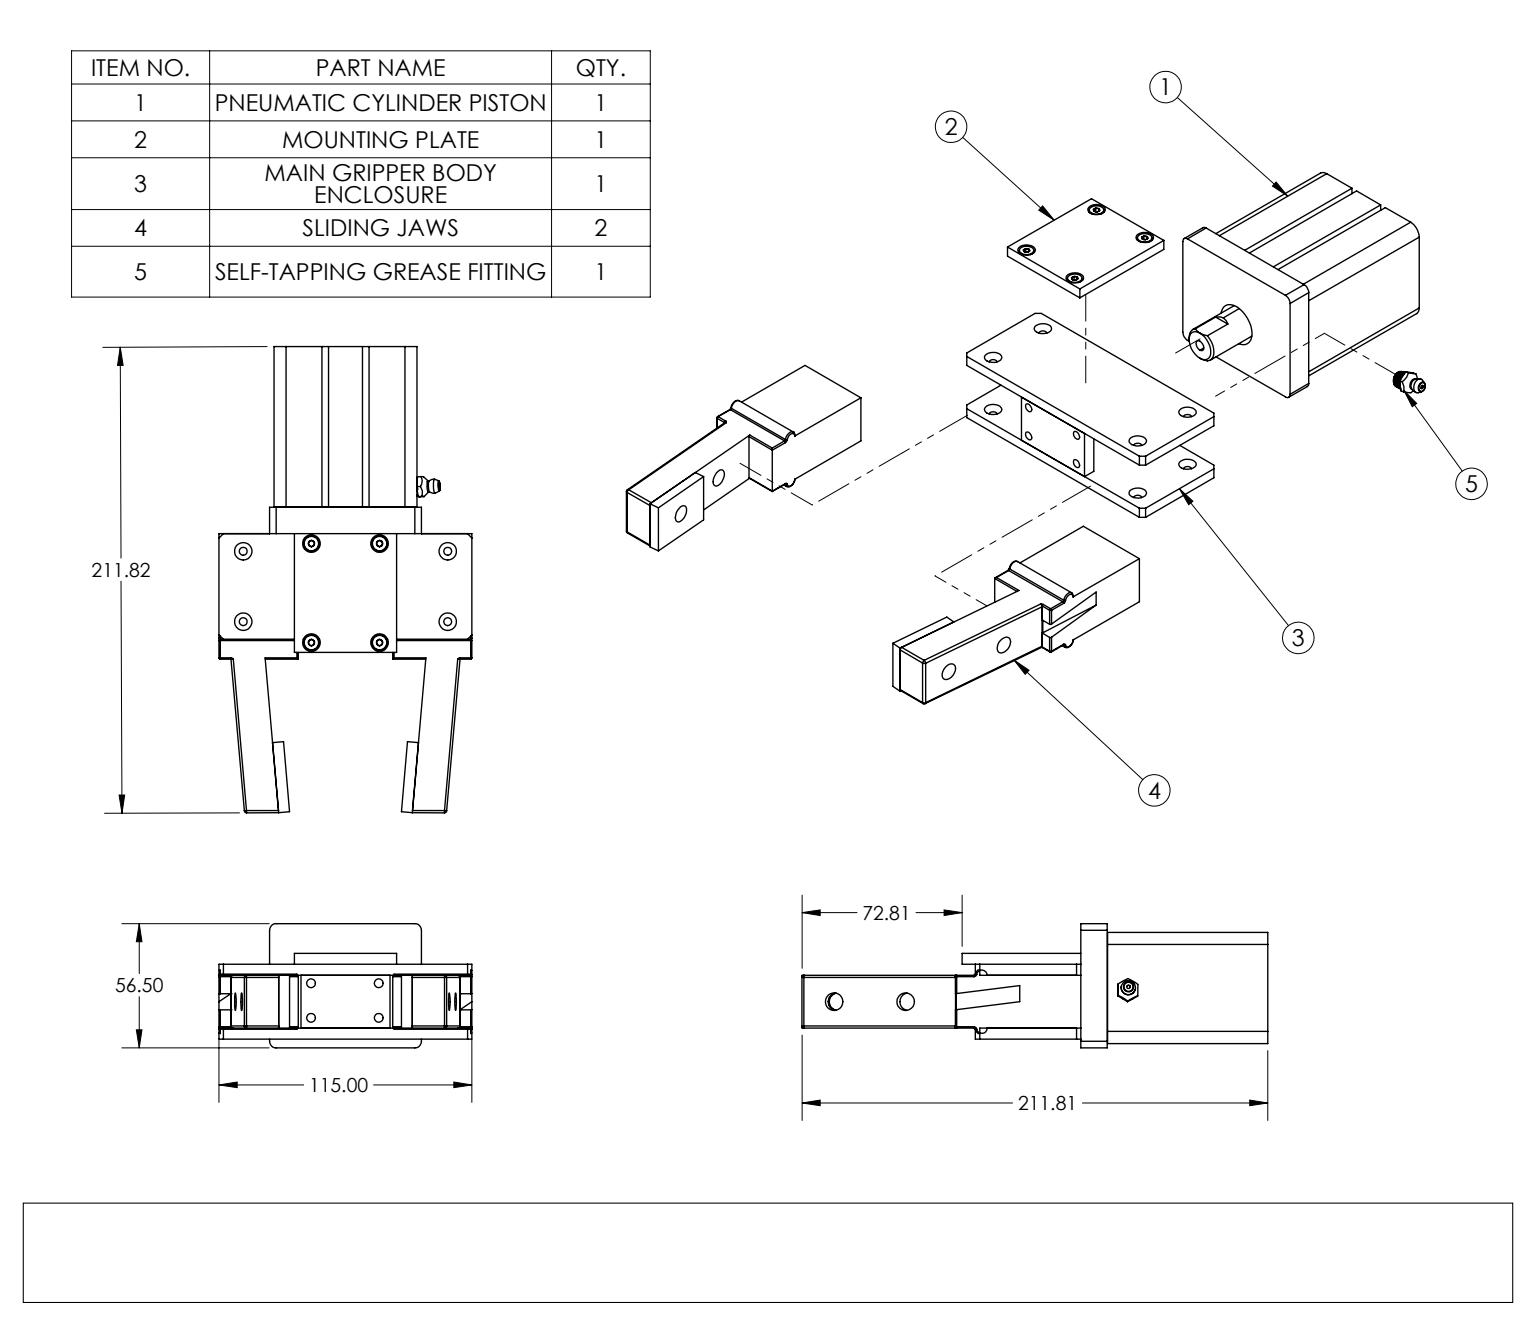
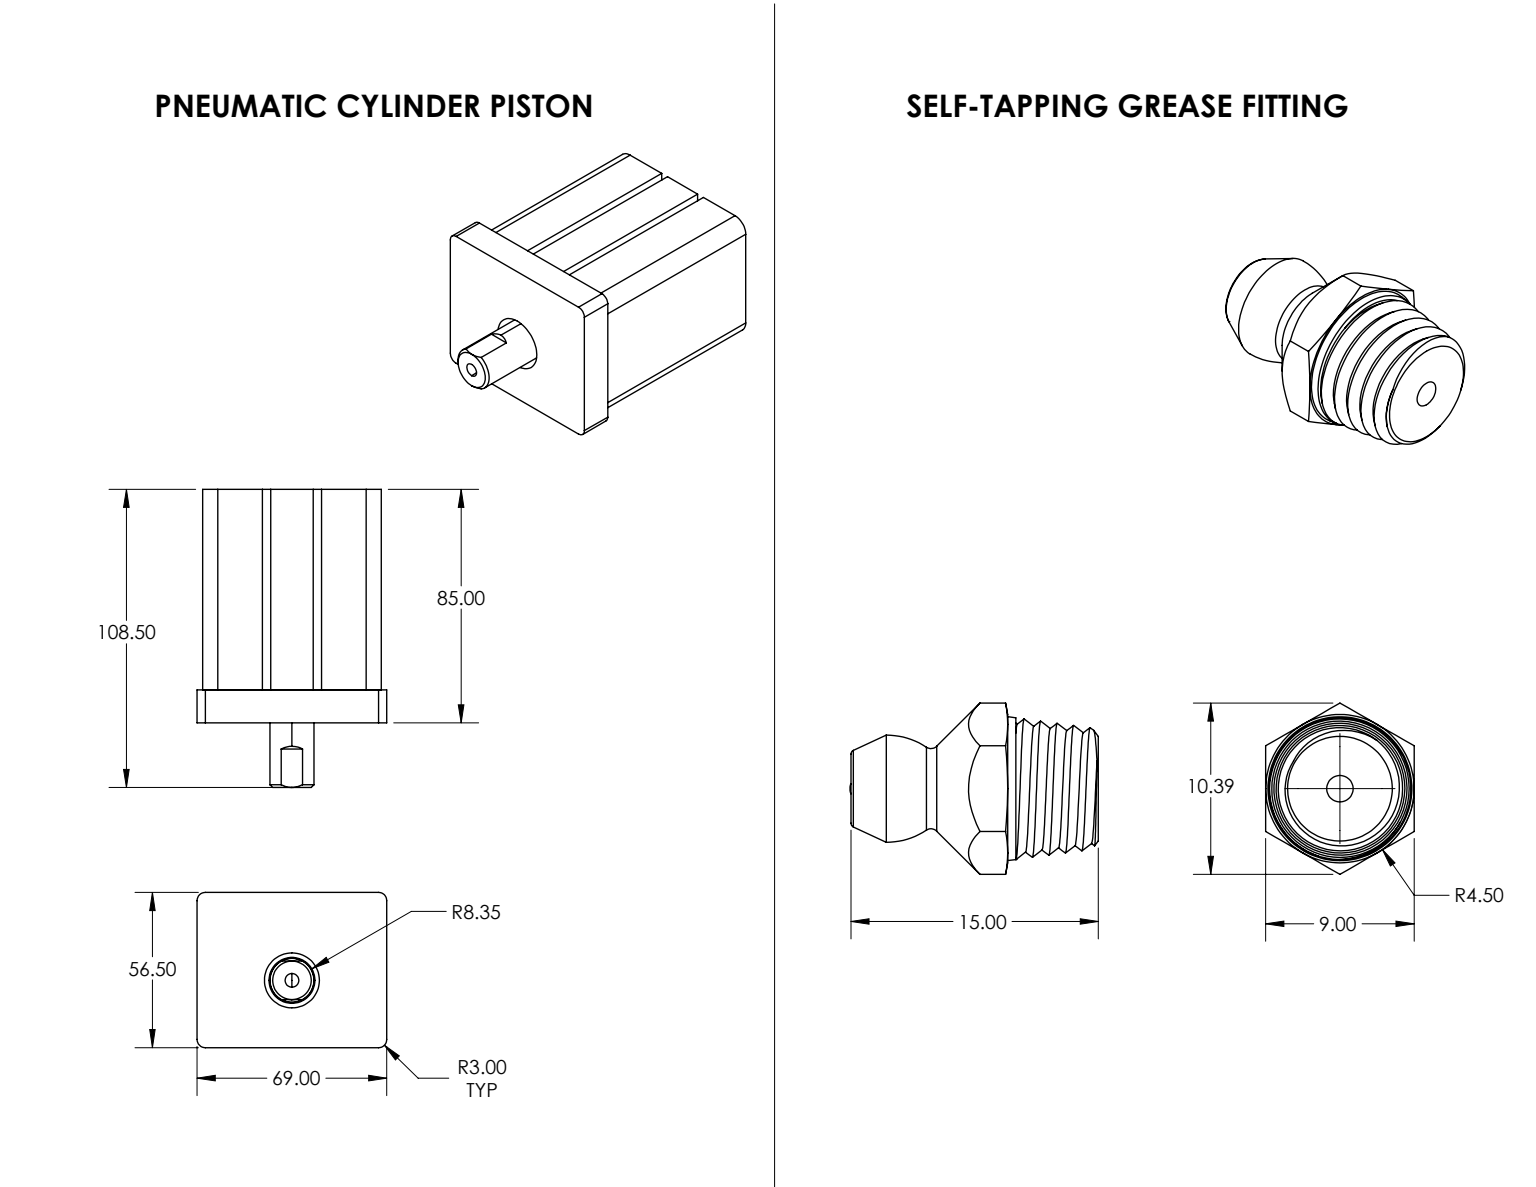
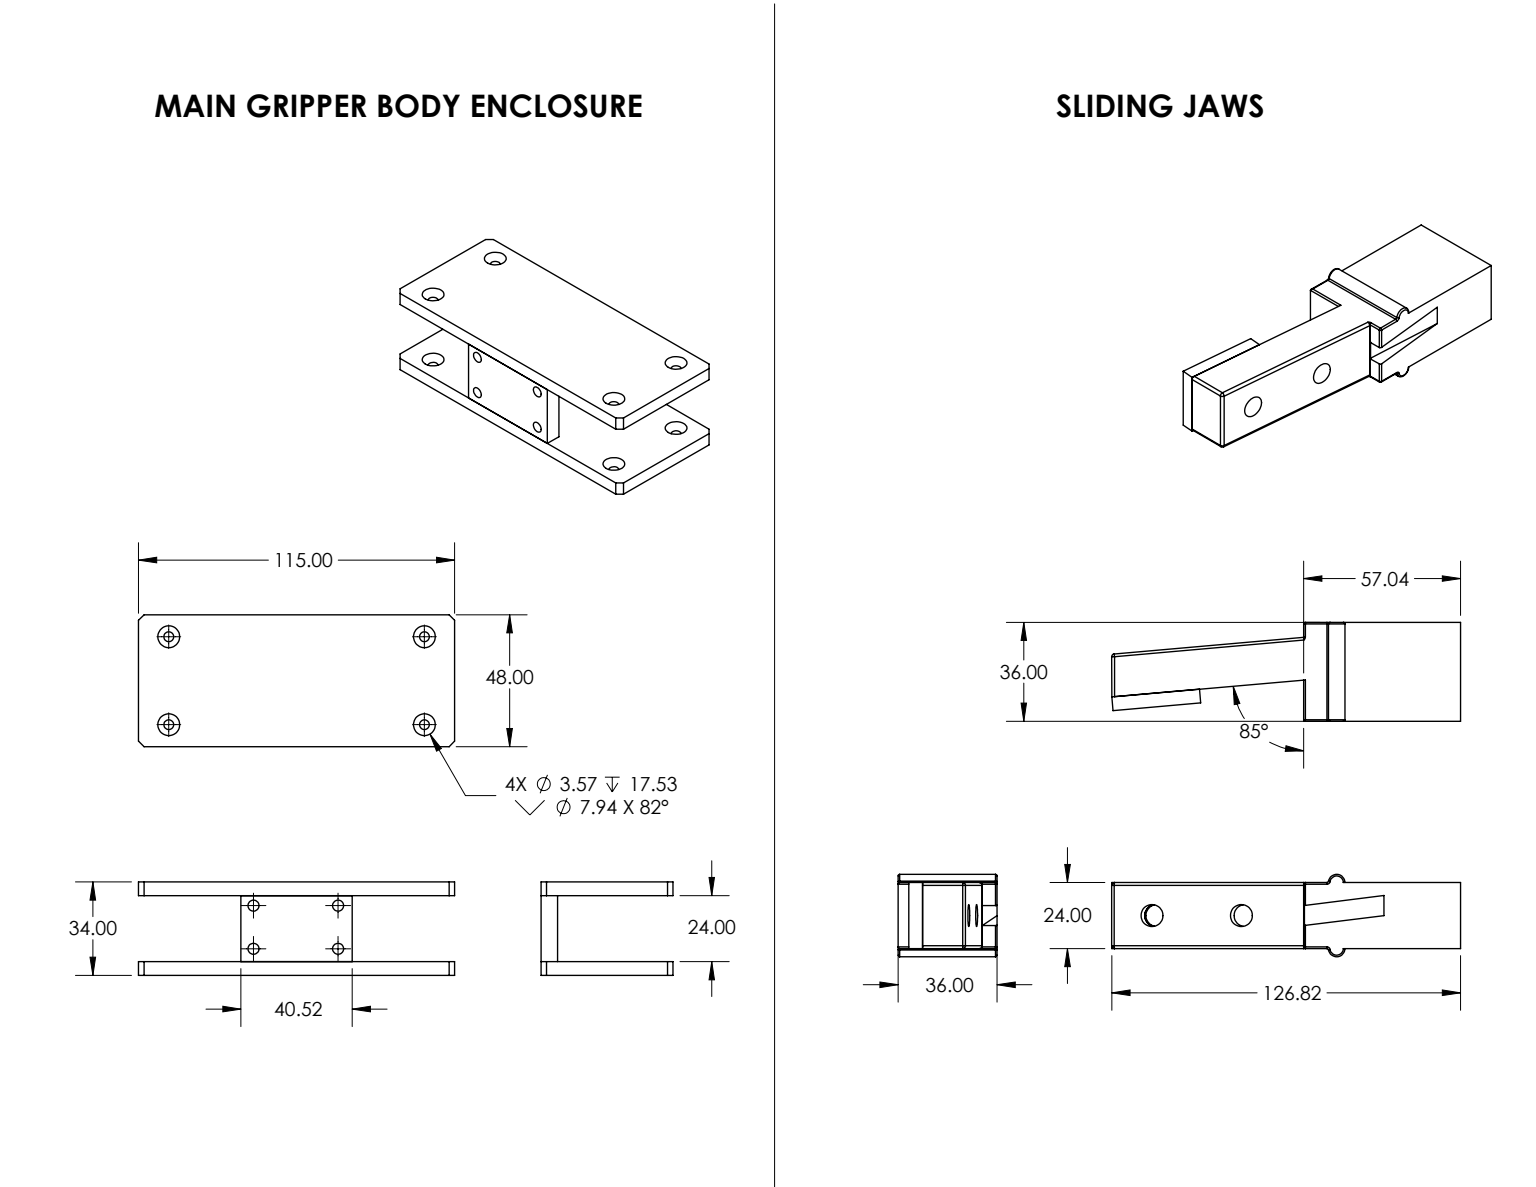
ISO-10303-21;
HEADER;
FILE_DESCRIPTION (('STEP AP214'),
    '1' );
FILE_NAME ('BR-Y-114',
    '2026-10-09T17:48:21',
    ( '' ),
    ( '' ),
    'SwSTEP 2.0',
    'SolidWorks 2024',
    '' );
FILE_SCHEMA (( 'AUTOMOTIVE_DESIGN' ));
ENDSEC;

DATA;
#1 = ORIENTED_EDGE ( 'NONE', *, *, #1535, .F. ) ;
#2 = ORIENTED_EDGE ( 'NONE', *, *, #10952, .T. ) ;
#3 = CARTESIAN_POINT ( 'NONE',  ( 2.229831107420913838, -3.725624999999957776, -2.719112200499452126 ) ) ;
#4 = EDGE_CURVE ( 'NONE', #455, #7951, #9514, .T. ) ;
#5 = CARTESIAN_POINT ( 'NONE',  ( -15.70313394609757296, -0.2715358723600092006, -23.82609623451302028 ) ) ;
#6 = DIRECTION ( 'NONE',  ( 0.000000000000000000, 1.000000000000000000, 0.000000000000000000 ) ) ;
#7 = DIRECTION ( 'NONE',  ( -1.000000000000000000, 0.000000000000000000, 0.000000000000000000 ) ) ;
#8 = FACE_OUTER_BOUND ( 'NONE', #14235, .T. ) ;
#9 = CARTESIAN_POINT ( 'NONE',  ( 4.499999999999994671, 2.375000000000011102, -5.510910596163089556E-16 ) ) ;
#10 = LINE ( 'NONE', #10400, #4062 ) ;
#11 = CARTESIAN_POINT ( 'NONE',  ( -48.27438362644000591, 99.17411849586700612, -145.4984795835769660 ) ) ;
#12 = DIRECTION ( 'NONE',  ( 0.000000000000000000, 0.000000000000000000, 1.000000000000000000 ) ) ;
#13 = DIRECTION ( 'NONE',  ( 0.8660254037844381525, 1.060575238724905436E-16, -0.5000000000000007772 ) ) ;
#14 = EDGE_LOOP ( 'NONE', ( #11433, #3957, #4882, #12655, #13949, #5070, #15047, #7038 ) ) ;
#15 = DIRECTION ( 'NONE',  ( 0.000000000000000000, 0.000000000000000000, 1.000000000000000000 ) ) ;
#16 = VERTEX_POINT ( 'NONE', #1531 ) ;
#17 = EDGE_LOOP ( 'NONE', ( #15211, #10608 ) ) ;
#18 = ADVANCED_FACE ( 'NONE', ( #1298 ), #7443, .F. ) ;
#19 = CARTESIAN_POINT ( 'NONE',  ( -3.913923972693154063, 0.4218750000000872080, 2.093842233512113626 ) ) ;
#20 = ORIENTED_EDGE ( 'NONE', *, *, #14135, .F. ) ;
#21 = CARTESIAN_POINT ( 'NONE',  ( -1.610069518889563289, -1.311713562373113096, -3.889976491222739252 ) ) ;
#22 = EDGE_CURVE ( 'NONE', #5823, #14725, #14225, .T. ) ;
#23 = DIRECTION ( 'NONE',  ( 0.000000000000000000, 0.000000000000000000, -1.000000000000000000 ) ) ;
#24 = CARTESIAN_POINT ( 'NONE',  ( 4.573385150445044900, -19.31989681812820692, 6.000000000000000000 ) ) ;
#25 = CIRCLE ( 'NONE', #1757, 2.000000000000001776 ) ;
#26 = CARTESIAN_POINT ( 'NONE',  ( 14.25000000000000000, -0.2038245569916330158, 23.22168783648699986 ) ) ;
#27 = EDGE_CURVE ( 'NONE', #14843, #4755, #2589, .T. ) ;
#28 = CARTESIAN_POINT ( 'NONE',  ( -69.77438362644001302, 82.17411849586700612, -29.37106258560738681 ) ) ;
#29 = ORIENTED_EDGE ( 'NONE', *, *, #8974, .F. ) ;
#30 = LINE ( 'NONE', #2442, #6868 ) ;
#31 = CIRCLE ( 'NONE', #14646, 3.499999999999999556 ) ;
#32 = APPLICATION_PROTOCOL_DEFINITION ( 'draft international standard', 'automotive_design', 1998, #9313 ) ;
#33 = ADVANCED_FACE ( 'NONE', ( #6140 ), #1221, .T. ) ;
#34 = ORIENTED_EDGE ( 'NONE', *, *, #12854, .F. ) ;
#35 = AXIS2_PLACEMENT_3D ( 'NONE', #11187, #8790, #2898 ) ;
#36 = CARTESIAN_POINT ( 'NONE',  ( 1.804739227294467563, -4.171875000000069278, -3.379404665904198968 ) ) ;
#37 = ORIENTED_EDGE ( 'NONE', *, *, #9789, .F. ) ;
#38 = VECTOR ( 'NONE', #447, 1000.000000000000114 ) ;
#39 = ADVANCED_FACE ( 'NONE', ( #3550 ), #5980, .T. ) ;
#40 = EDGE_CURVE ( 'NONE', #11360, #1952, #11269, .T. ) ;
#41 = CARTESIAN_POINT ( 'NONE',  ( 15.50000000000000000, -0.4000000000000000222, -22.50000000000000000 ) ) ;
#42 = CARTESIAN_POINT ( 'NONE',  ( -1.024675879034753434, -5.362115055319378598, 3.196030698784670054 ) ) ;
#43 = AXIS2_PLACEMENT_3D ( 'NONE', #8460, #2484, #4677 ) ;
#44 = LINE ( 'NONE', #15319, #14958 ) ;
#45 = EDGE_CURVE ( 'NONE', #7802, #1067, #10681, .T. ) ;
#46 = CARTESIAN_POINT ( 'NONE',  ( 3.469446951953614189E-15, -24.00000000000000000, 0.000000000000000000 ) ) ;
#47 = CARTESIAN_POINT ( 'NONE',  ( 3.443564157863920006, -5.257675013607999936, 0.5807209424340332715 ) ) ;
#48 = LINE ( 'NONE', #15323, #3608 ) ;
#49 = VECTOR ( 'NONE', #15077, 1000.000000000000000 ) ;
#50 = CARTESIAN_POINT ( 'NONE',  ( 1.634139617129772404, -12.00000029085424025, -0.3335879563140197179 ) ) ;
#51 = VERTEX_POINT ( 'NONE', #8286 ) ;
#52 = FACE_OUTER_BOUND ( 'NONE', #854, .T. ) ;
#53 = EDGE_CURVE ( 'NONE', #8592, #3175, #10509, .T. ) ;
#54 = ORIENTED_EDGE ( 'NONE', *, *, #8192, .T. ) ;
#55 = CARTESIAN_POINT ( 'NONE',  ( -22.96690797774568082, 1.660051434983101380E-15, 52.36213013816526285 ) ) ;
#56 = CARTESIAN_POINT ( 'NONE',  ( 0.3421672931281763419, -3.819374999999898268, -3.487344533451359307 ) ) ;
#57 = ORIENTED_EDGE ( 'NONE', *, *, #8169, .T. ) ;
#58 = ORIENTED_EDGE ( 'NONE', *, *, #11069, .T. ) ;
#59 = VERTEX_POINT ( 'NONE', #14253 ) ;
#60 = VECTOR ( 'NONE', #13397, 1000.000000000000000 ) ;
#61 = CARTESIAN_POINT ( 'NONE',  ( -52.77438362643999881, 65.17411849586700612, -149.9984795835770228 ) ) ;
#62 = DIRECTION ( 'NONE',  ( 0.000000000000000000, 0.000000000000000000, -1.000000000000000000 ) ) ;
#63 = LINE ( 'NONE', #5245, #7516 ) ;
#64 = CARTESIAN_POINT ( 'NONE',  ( -14.25000000000000000, -2.500000000000000000, -23.22168783648699986 ) ) ;
#65 = CARTESIAN_POINT ( 'NONE',  ( -96.77438362643999881, 110.1741184958670061, -15.85886927678779834 ) ) ;
#66 = DIRECTION ( 'NONE',  ( -0.8660254037844482555, 0.000000000000000000, 0.4999999999999831801 ) ) ;
#67 = CARTESIAN_POINT ( 'NONE',  ( -3.325293793763300698, -4.038125000000090559, -1.009645679448947231 ) ) ;
#68 = DIRECTION ( 'NONE',  ( -1.000000000000000000, 0.000000000000000000, 0.000000000000000000 ) ) ;
#69 = ORIENTED_EDGE ( 'NONE', *, *, #2752, .F. ) ;
#70 = AXIS2_PLACEMENT_3D ( 'NONE', #89, #11892, #6017 ) ;
#71 = VERTEX_POINT ( 'NONE', #12157 ) ;
#72 = ORIENTED_EDGE ( 'NONE', *, *, #1086, .F. ) ;
#73 = EDGE_LOOP ( 'NONE', ( #5706, #14466 ) ) ;
#74 = VECTOR ( 'NONE', #15192, 1000.000000000000000 ) ;
#75 = CARTESIAN_POINT ( 'NONE',  ( -1.054465238365572599, -2.881875000000049702, -3.471494129216005753 ) ) ;
#76 = CARTESIAN_POINT ( 'NONE',  ( -15.91242688423474050, -0.3152598339554945062, -23.70526090034005051 ) ) ;
#77 = CARTESIAN_POINT ( 'NONE',  ( 15.50000000000000000, -2.500000000000000000, -21.05662432702600029 ) ) ;
#78 = VECTOR ( 'NONE', #4596, 1000.000000000000000 ) ;
#79 = CARTESIAN_POINT ( 'NONE',  ( -66.41143315690761995, 66.60412428008086749, -81.84847958357697451 ) ) ;
#80 = AXIS2_PLACEMENT_3D ( 'NONE', #7760, #5130, #12410 ) ;
#81 = CARTESIAN_POINT ( 'NONE',  ( -46.58670980944423690, 5.000000000000000000, 89.50956111919107627 ) ) ;
#82 = CARTESIAN_POINT ( 'NONE',  ( 1.375881166777175254E-16, 9.250000000000000000, 0.000000000000000000 ) ) ;
#83 = CARTESIAN_POINT ( 'NONE',  ( 5.196152422706631135, 0.1227504548087541975, -1.122964458370237425E-15 ) ) ;
#84 = DIRECTION ( 'NONE',  ( 0.000000000000000000, 0.000000000000000000, -1.000000000000000000 ) ) ;
#85 = CARTESIAN_POINT ( 'NONE',  ( -14.66434062215826017, -0.3156604612126701626, -21.53909249377373669 ) ) ;
#86 = CARTESIAN_POINT ( 'NONE',  ( -52.77438362644100067, 101.5320169952374414, -147.9984795835769944 ) ) ;
#87 = AXIS2_PLACEMENT_3D ( 'NONE', #15229, #11833, #9343 ) ;
#88 = ORIENTED_EDGE ( 'NONE', *, *, #3312, .F. ) ;
#89 = CARTESIAN_POINT ( 'NONE',  ( 23.77513017582411692, -1.718469852516944459E-15, 56.45152858669899132 ) ) ;
#90 = ADVANCED_FACE ( 'NONE', ( #3635 ), #13178, .F. ) ;
#91 = EDGE_LOOP ( 'NONE', ( #13026, #11376, #12527, #2577 ) ) ;
#92 = ORIENTED_EDGE ( 'NONE', *, *, #11605, .T. ) ;
#93 = AXIS2_PLACEMENT_3D ( 'NONE', #13950, #3324, #14805 ) ;
#94 = VECTOR ( 'NONE', #206, 1000.000000000000114 ) ;
#95 = CARTESIAN_POINT ( 'NONE',  ( 0.4342252132666136744, 0.2343749999999768518, 4.392589664459995547 ) ) ;
#96 = ORIENTED_EDGE ( 'NONE', *, *, #11121, .T. ) ;
#97 = CARTESIAN_POINT ( 'NONE',  ( 0.8081574754459883714, -1.780463562373038489, 4.068519560952849723 ) ) ;
#98 = DIRECTION ( 'NONE',  ( 0.000000000000000000, 1.000000000000000000, 0.000000000000000000 ) ) ;
#99 = PLANE ( 'NONE',  #8327 ) ;
#100 = DIRECTION ( 'NONE',  ( 0.000000000000000000, -1.445602896647339508E-15, -1.000000000000000000 ) ) ;
#101 = AXIS2_PLACEMENT_3D ( 'NONE', #55, #7289, #9436 ) ;
#102 = AXIS2_PLACEMENT_3D ( 'NONE', #7303, #5128, #12107 ) ;
#103 = ADVANCED_FACE ( 'NONE', ( #4721 ), #2539, .F. ) ;
#104 = AXIS2_PLACEMENT_3D ( 'NONE', #9818, #12003, #8653 ) ;
#105 = CARTESIAN_POINT ( 'NONE',  ( -55.27438362644100067, 99.17411849586700612, -145.2984795835770058 ) ) ;
#106 = ORIENTED_EDGE ( 'NONE', *, *, #3872, .T. ) ;
#107 = CARTESIAN_POINT ( 'NONE',  ( -89.52438362644001302, 99.17411849586700612, -86.49847958357699440 ) ) ;
#108 = ADVANCED_FACE ( 'NONE', ( #11856, #8368 ), #12015, .T. ) ;
#109 = LINE ( 'NONE', #5963, #14166 ) ;
#110 = ORIENTED_EDGE ( 'NONE', *, *, #7891, .F. ) ;
#111 = DIRECTION ( 'NONE',  ( -0.7071067811865470176, -0.7071067811865481278, 0.000000000000000000 ) ) ;
#112 = CARTESIAN_POINT ( 'NONE',  ( 0.001419932108912198322, -3.750000000000078160, 3.886924930609184869 ) ) ;
#113 = ORIENTED_EDGE ( 'NONE', *, *, #13222, .F. ) ;
#114 = B_SPLINE_CURVE_WITH_KNOTS ( 'NONE', 3,
 ( #8146, #5687, #3332, #849 ),
 .UNSPECIFIED., .F., .F.,
 ( 4, 4 ),
 ( 0.000000000000000000, 1.000000000000000000 ),
 .UNSPECIFIED. ) ;
#115 = AXIS2_PLACEMENT_3D ( 'NONE', #6388, #13511, #12041 ) ;
#116 = AXIS2_PLACEMENT_3D ( 'NONE', #9604, #4733, #11793 ) ;
#117 = CARTESIAN_POINT ( 'NONE',  ( 3.639928100339127948, -0.5225000000000105116, 1.508827519571796172 ) ) ;
#118 = CARTESIAN_POINT ( 'NONE',  ( 0.2965589474581596385, -5.389768145603638594, 3.307028203814240008 ) ) ;
#119 = EDGE_CURVE ( 'NONE', #467, #14870, #5816, .T. ) ;
#120 = LINE ( 'NONE', #3929, #1107 ) ;
#121 = FACE_OUTER_BOUND ( 'NONE', #4343, .T. ) ;
#122 = FACE_OUTER_BOUND ( 'NONE', #15028, .T. ) ;
#123 = DIRECTION ( 'NONE',  ( 0.000000000000000000, 1.000000000000000000, 0.000000000000000000 ) ) ;
#124 = CIRCLE ( 'NONE', #5857, 3.750000000000003553 ) ;
#125 = EDGE_CURVE ( 'NONE', #14595, #12756, #14394, .T. ) ;
#126 = STYLED_ITEM ( 'NONE', ( #12347 ), #5610 ) ;
#127 = EDGE_LOOP ( 'NONE', ( #6019, #5479, #5692, #8354 ) ) ;
#128 = AXIS2_PLACEMENT_3D ( 'NONE', #1233, #11714, #2169 ) ;
#129 = DIRECTION ( 'NONE',  ( 0.000000000000000000, 0.000000000000000000, 1.000000000000000000 ) ) ;
#130 = ORIENTED_EDGE ( 'NONE', *, *, #9024, .T. ) ;
#131 = ORIENTED_EDGE ( 'NONE', *, *, #12812, .T. ) ;
#132 = CARTESIAN_POINT ( 'NONE',  ( 2.822884439542550084, -2.694375000000075460, -2.318423337397389705 ) ) ;
#133 = EDGE_LOOP ( 'NONE', ( #9596, #14625, #7458, #244 ) ) ;
#134 = VERTEX_POINT ( 'NONE', #5029 ) ;
#135 = ORIENTED_EDGE ( 'NONE', *, *, #4809, .F. ) ;
#136 = EDGE_CURVE ( 'NONE', #3919, #16, #2769, .T. ) ;
#137 = EDGE_CURVE ( 'NONE', #3871, #7132, #3941, .T. ) ;
#138 = VECTOR ( 'NONE', #8882, 1000.000000000000000 ) ;
#139 = CARTESIAN_POINT ( 'NONE',  ( -16.75000000000000000, -2.500000000000000000, -23.22168783648699986 ) ) ;
#140 = AXIS2_PLACEMENT_3D ( 'NONE', #12539, #11367, #14918 ) ;
#141 = AXIS2_PLACEMENT_3D ( 'NONE', #9942, #7412, #9791 ) ;
#142 = DIRECTION ( 'NONE',  ( 1.000000000000000000, 0.000000000000000000, 0.000000000000000000 ) ) ;
#143 = EDGE_CURVE ( 'NONE', #10494, #8073, #2934, .T. ) ;
#144 = CARTESIAN_POINT ( 'NONE',  ( -52.77438362643999881, 67.53201699523744139, -147.9984795835769944 ) ) ;
#145 = CARTESIAN_POINT ( 'NONE',  ( -3.897114317029972685, -9.945166405816852549E-15, -2.249999999999999112 ) ) ;
#146 =( NAMED_UNIT ( * ) SI_UNIT ( $, .STERADIAN. ) SOLID_ANGLE_UNIT ( ) );
#147 = CARTESIAN_POINT ( 'NONE',  ( 22.58164641901421632, -12.60000029085423812, -8.183940086454239093 ) ) ;
#148 = CARTESIAN_POINT ( 'NONE',  ( 3.520079602834293109, -3.569375000000153619, 0.3476102605345692265 ) ) ;
#149 = EDGE_CURVE ( 'NONE', #14279, #1795, #4826, .T. ) ;
#150 = FACE_OUTER_BOUND ( 'NONE', #9608, .T. ) ;
#151 = EDGE_CURVE ( 'NONE', #8289, #4668, #11363, .T. ) ;
#152 = ORIENTED_EDGE ( 'NONE', *, *, #14283, .F. ) ;
#153 = CARTESIAN_POINT ( 'NONE',  ( -86.77438362643999881, 67.53201699523744139, -150.4984795835770228 ) ) ;
#154 = VECTOR ( 'NONE', #6765, 1000.000000000000000 ) ;
#155 = ORIENTED_EDGE ( 'NONE', *, *, #10965, .T. ) ;
#156 = CIRCLE ( 'NONE', #9319, 2.750000000000002665 ) ;
#157 = EDGE_LOOP ( 'NONE', ( #11724, #9065, #934, #14643 ) ) ;
#158 = EDGE_LOOP ( 'NONE', ( #13988, #8666, #2521, #1723 ) ) ;
#159 = VECTOR ( 'NONE', #3125, 1000.000000000000000 ) ;
#160 = VERTEX_POINT ( 'NONE', #3006 ) ;
#161 =( NAMED_UNIT ( * ) SI_UNIT ( $, .STERADIAN. ) SOLID_ANGLE_UNIT ( ) );
#162 = CARTESIAN_POINT ( 'NONE',  ( -0.001340710925747373022, -2.834999999999994635, -3.634308738048381393 ) ) ;
#163 = PRODUCT_DEFINITION_SHAPE ( 'NONE', 'NONE',  #15338 ) ;
#164 = DIRECTION ( 'NONE',  ( -0.9375000000000006661, 0.000000000000000000, -0.3479852726768744020 ) ) ;
#165 = CARTESIAN_POINT ( 'NONE',  ( 2.937061643673781752, -5.103115294876279684, -2.234448363260541193 ) ) ;
#166 = DIRECTION ( 'NONE',  ( 0.000000000000000000, -0.000000000000000000, 1.000000000000000000 ) ) ;
#167 = CARTESIAN_POINT ( 'NONE',  ( -13.41835358098578723, 11.39999970914575833, 0.2664120436859911956 ) ) ;
#168 = AXIS2_PLACEMENT_3D ( 'NONE', #2465, #7215, #142 ) ;
#169 = DIRECTION ( 'NONE',  ( -9.035018104045795506E-17, -0.9860132971832696880, -0.1666666666666656860 ) ) ;
#170 = FACE_OUTER_BOUND ( 'NONE', #13767, .T. ) ;
#171 = CARTESIAN_POINT ( 'NONE',  ( -86.77438362644100778, 101.5320169952374414, -147.9984795835769944 ) ) ;
#172 = CARTESIAN_POINT ( 'NONE',  ( -86.77438362644100778, 96.81621999649657084, -150.4984795835770228 ) ) ;
#173 = FACE_OUTER_BOUND ( 'NONE', #7801, .T. ) ;
#174 = ORIENTED_EDGE ( 'NONE', *, *, #12843, .T. ) ;
#175 = DIRECTION ( 'NONE',  ( -0.000000000000000000, 1.000000000000000000, 4.336808689942017736E-16 ) ) ;
#176 = EDGE_LOOP ( 'NONE', ( #13806, #13422, #10645, #9844 ) ) ;
#177 = EDGE_LOOP ( 'NONE', ( #7583, #9630, #5793, #14257 ) ) ;
#178 = DIRECTION ( 'NONE',  ( 0.000000000000000000, 1.000000000000000000, 0.000000000000000000 ) ) ;
#179 = AXIS2_PLACEMENT_3D ( 'NONE', #10567, #13983, #7013 ) ;
#180 = VECTOR ( 'NONE', #527, 1000.000000000000000 ) ;
#181 = VERTEX_POINT ( 'NONE', #14626 ) ;
#182 = CARTESIAN_POINT ( 'NONE',  ( 2.923540125992261984, -1.874213562373038489, 2.925090027579059004 ) ) ;
#183 = CARTESIAN_POINT ( 'NONE',  ( -15.50000000000000000, -5.000000000000000000, -22.50000000000000000 ) ) ;
#184 = CARTESIAN_POINT ( 'NONE',  ( -89.27438362644100778, 99.17411849586700612, -182.2484795835770228 ) ) ;
#185 = FACE_OUTER_BOUND ( 'NONE', #11001, .T. ) ;
#186 = CIRCLE ( 'NONE', #13087, 4.000000000000000000 ) ;
#187 = FACE_OUTER_BOUND ( 'NONE', #12629, .T. ) ;
#188 = VERTEX_POINT ( 'NONE', #368 ) ;
#189 = CARTESIAN_POINT ( 'NONE',  ( 15.50000000000000000, -0.4000000000000000222, 25.99999999999999645 ) ) ;
#190 = APPLICATION_PROTOCOL_DEFINITION ( 'draft international standard', 'automotive_design', 1998, #4867 ) ;
#191 = VERTEX_POINT ( 'NONE', #7522 ) ;
#192 = CARTESIAN_POINT ( 'NONE',  ( -1.106373576938931125, -4.296874999999863221, -3.650653549769442119 ) ) ;
#193 = ORIENTED_EDGE ( 'NONE', *, *, #14265, .T. ) ;
#194 = EDGE_CURVE ( 'NONE', #3175, #4923, #10253, .T. ) ;
#195 = CIRCLE ( 'NONE', #7158, 5.500000000000005329 ) ;
#196 = CARTESIAN_POINT ( 'NONE',  ( 3.459076575081923899, -0.6631250000000769029, -1.847748348019847109 ) ) ;
#197 = EDGE_CURVE ( 'NONE', #3708, #3101, #10343, .T. ) ;
#198 = CARTESIAN_POINT ( 'NONE',  ( -2.819918635305147525, -5.316771972388096401, 1.943909394665495727 ) ) ;
#199 = CARTESIAN_POINT ( 'NONE',  ( 57.41329019055577021, 5.000000000000001776, 97.50956111919106206 ) ) ;
#200 = DIRECTION ( 'NONE',  ( 0.000000000000000000, 0.1240337885538713436, -0.9922779949676268085 ) ) ;
#201 = CARTESIAN_POINT ( 'NONE',  ( -88.81638362644000040, 63.99516924618178848, -147.9984795835769944 ) ) ;
#202 = CARTESIAN_POINT ( 'NONE',  ( -69.77438362644100778, 72.17411849586700612, -67.49847958357700861 ) ) ;
#203 = DIRECTION ( 'NONE',  ( 0.000000000000000000, 1.000000000000000000, 0.000000000000000000 ) ) ;
#204 = VECTOR ( 'NONE', #14939, 1000.000000000000114 ) ;
#205 = EDGE_LOOP ( 'NONE', ( #7542, #9169, #8571, #7456 ) ) ;
#206 = DIRECTION ( 'NONE',  ( 0.7071067811865451302, -0.000000000000000000, -0.7071067811865500152 ) ) ;
#207 = DIRECTION ( 'NONE',  ( 0.000000000000000000, 0.000000000000000000, 1.000000000000000000 ) ) ;
#208 = ORIENTED_EDGE ( 'NONE', *, *, #4156, .T. ) ;
#209 = DIRECTION ( 'NONE',  ( 0.000000000000000000, -1.000000000000000000, 0.000000000000000000 ) ) ;
#210 = CARTESIAN_POINT ( 'NONE',  ( 2.488663048653546372, -3.709999999999854303, -2.487386788893799938 ) ) ;
#211 = ORIENTED_EDGE ( 'NONE', *, *, #10659, .T. ) ;
#212 = ADVANCED_FACE ( 'NONE', ( #8971 ), #14705, .T. ) ;
#213 = EDGE_LOOP ( 'NONE', ( #14069, #5865 ) ) ;
#214 = EDGE_CURVE ( 'NONE', #71, #6831, #12240, .T. ) ;
#215 = VERTEX_POINT ( 'NONE', #12398 ) ;
#216 = CIRCLE ( 'NONE', #8155, 3.499999999999999556 ) ;
#217 = DIRECTION ( 'NONE',  ( 1.000000000000000000, 0.000000000000000000, 0.000000000000000000 ) ) ;
#218 = FACE_OUTER_BOUND ( 'NONE', #9920, .T. ) ;
#219 = CARTESIAN_POINT ( 'NONE',  ( -23.24999999999999645, -5.000000000000000000, 2.987579319737834353E-15 ) ) ;
#220 = FACE_BOUND ( 'NONE', #13407, .T. ) ;
#221 = CARTESIAN_POINT ( 'NONE',  ( -90.52438362644100778, 99.17411849586700612, -150.4984795835770228 ) ) ;
#222 = CARTESIAN_POINT ( 'NONE',  ( 3.376561219002149450, -3.631875000000035048, -1.025635141340205836 ) ) ;
#223 = CARTESIAN_POINT ( 'NONE',  ( 22.58164641901421277, 7.308633194218583817, -28.96834603255778262 ) ) ;
#224 = EDGE_CURVE ( 'NONE', #8420, #5168, #5339, .T. ) ;
#225 = ORIENTED_EDGE ( 'NONE', *, *, #3832, .T. ) ;
#226 = ORIENTED_EDGE ( 'NONE', *, *, #4376, .F. ) ;
#227 = ORIENTED_EDGE ( 'NONE', *, *, #3079, .F. ) ;
#228 = EDGE_LOOP ( 'NONE', ( #12564, #488 ) ) ;
#229 = ORIENTED_EDGE ( 'NONE', *, *, #14616, .F. ) ;
#230 = EDGE_CURVE ( 'NONE', #5514, #2409, #14717, .T. ) ;
#231 = CARTESIAN_POINT ( 'NONE',  ( 2.255458548909140770, -3.444374999999939568, 2.746210667320699184 ) ) ;
#232 = EDGE_CURVE ( 'NONE', #1220, #5341, #3328, .T. ) ;
#233 = ADVANCED_FACE ( 'NONE', ( #7744 ), #2100, .F. ) ;
#234 = FILL_AREA_STYLE ('',( #7467 ) ) ;
#235 = PLANE ( 'NONE',  #9452 ) ;
#236 = DIRECTION ( 'NONE',  ( -0.000000000000000000, 0.000000000000000000, 1.000000000000000000 ) ) ;
#237 = CARTESIAN_POINT ( 'NONE',  ( 10.10045295220800554, 10.99999970914572778, 70.08978589960025829 ) ) ;
#238 = CARTESIAN_POINT ( 'NONE',  ( -44.58670980944422269, 5.000000000000000000, 89.50956111919107627 ) ) ;
#239 = DIRECTION ( 'NONE',  ( -0.000000000000000000, 0.000000000000000000, -1.000000000000000000 ) ) ;
#240 = LINE ( 'NONE', #14588, #11040 ) ;
#241 = DIRECTION ( 'NONE',  ( -1.000000000000000000, 0.000000000000000000, 0.000000000000000000 ) ) ;
#242 = CARTESIAN_POINT ( 'NONE',  ( -84.02438362643999881, 65.17411849586700612, -86.49847958357699440 ) ) ;
#243 = EDGE_CURVE ( 'NONE', #3902, #13427, #9900, .T. ) ;
#244 = ORIENTED_EDGE ( 'NONE', *, *, #1570, .T. ) ;
#245 = DIRECTION ( 'NONE',  ( 0.000000000000000000, -1.000000000000000000, 0.000000000000000000 ) ) ;
#246 = ORIENTED_EDGE ( 'NONE', *, *, #2791, .T. ) ;
#247 = EDGE_LOOP ( 'NONE', ( #5782, #13390 ) ) ;
#248 = CARTESIAN_POINT ( 'NONE',  ( 3.211975673186791891, -5.553749999999917364, 0.6376497042497289991 ) ) ;
#249 = EDGE_CURVE ( 'NONE', #6663, #9914, #13638, .T. ) ;
#250 = CARTESIAN_POINT ( 'NONE',  ( -2.085189712146006347, 0.3281249999999837907, 3.904486635941227579 ) ) ;
#251 = CARTESIAN_POINT ( 'NONE',  ( -4.010609860205056165, -1.452338562373114650, -1.217768749654296601 ) ) ;
#252 = DIRECTION ( 'NONE',  ( 0.000000000000000000, 1.000000000000000000, 0.000000000000000000 ) ) ;
#253 = CYLINDRICAL_SURFACE ( 'NONE', #1029, 4.000000000000000000 ) ;
#254 = B_SPLINE_CURVE_WITH_KNOTS ( 'NONE', 3,
 ( #13370, #13070, #7240, #85, #9698, #9626 ),
 .UNSPECIFIED., .F., .F.,
 ( 4, 2, 4 ),
 ( 0.0002380763768129734448, 0.7291065797294584705, 1.457975083082104106 ),
 .UNSPECIFIED. ) ;
#255 = DIRECTION ( 'NONE',  ( 0.000000000000000000, 0.000000000000000000, -1.000000000000000000 ) ) ;
#256 = DIRECTION ( 'NONE',  ( 0.000000000000000000, 0.000000000000000000, 1.000000000000000000 ) ) ;
#257 = DIRECTION ( 'NONE',  ( 0.000000000000000000, 0.000000000000000000, -1.000000000000000000 ) ) ;
#258 = ORIENTED_EDGE ( 'NONE', *, *, #13416, .T. ) ;
#259 = CARTESIAN_POINT ( 'NONE',  ( -86.77438362644100778, 101.5320169952374414, -147.9984795835769944 ) ) ;
#260 = ORIENTED_EDGE ( 'NONE', *, *, #8838, .T. ) ;
#261 = FILL_AREA_STYLE_COLOUR ( '', #11287 ) ;
#262 = CARTESIAN_POINT ( 'NONE',  ( -2.390027884620886667, -4.640624999999809042, 2.914437415443186907 ) ) ;
#263 = VERTEX_POINT ( 'NONE', #12551 ) ;
#264 = CARTESIAN_POINT ( 'NONE',  ( 3.447003937676299312, -4.936713562372625042, 1.426311973487309981 ) ) ;
#265 = CIRCLE ( 'NONE', #4742, 9.999999999999994671 ) ;
#266 = DIRECTION ( 'NONE',  ( 0.000000000000000000, 1.000000000000000000, 0.000000000000000000 ) ) ;
#267 = CARTESIAN_POINT ( 'NONE',  ( -59.02799568714584666, 164.3482369917340122, -79.59847958357700293 ) ) ;
#268 = LINE ( 'NONE', #10989, #10255 ) ;
#269 = DIRECTION ( 'NONE',  ( 0.000000000000000000, -1.000000000000000000, 0.000000000000000000 ) ) ;
#270 = CARTESIAN_POINT ( 'NONE',  ( -73.76311196519618818, 67.29799558322736175, -81.84847958357697451 ) ) ;
#271 = DIRECTION ( 'NONE',  ( 1.000000000000000000, 0.000000000000000000, 0.000000000000000000 ) ) ;
#272 = CARTESIAN_POINT ( 'NONE',  ( 15.50000000000000000, 0.000000000000000000, 22.50000000000000000 ) ) ;
#273 = PLANE ( 'NONE',  #3768 ) ;
#274 = CIRCLE ( 'NONE', #12179, 17.85000000000000497 ) ;
#275 = ORIENTED_EDGE ( 'NONE', *, *, #2044, .F. ) ;
#276 = LINE ( 'NONE', #5026, #94 ) ;
#277 = EDGE_CURVE ( 'NONE', #4210, #1225, #6107, .T. ) ;
#278 = ORIENTED_EDGE ( 'NONE', *, *, #3265, .F. ) ;
#279 = CARTESIAN_POINT ( 'NONE',  ( -75.01311196519617397, 67.29799558322736175, -83.44847958357698303 ) ) ;
#280 = CARTESIAN_POINT ( 'NONE',  ( 1.342127543875233808, -3.772500000000060805, -3.243584335895733251 ) ) ;
#281 = ORIENTED_EDGE ( 'NONE', *, *, #748, .F. ) ;
#282 = EDGE_LOOP ( 'NONE', ( #3121, #10852 ) ) ;
#283 = ORIENTED_EDGE ( 'NONE', *, *, #13080, .F. ) ;
#284 = CARTESIAN_POINT ( 'NONE',  ( -48.27438362644000591, 99.17411849586700612, -145.4984795835769660 ) ) ;
#285 = AXIS2_PLACEMENT_3D ( 'NONE', #3423, #3496, #1409 ) ;
#286 = CARTESIAN_POINT ( 'NONE',  ( -0.9158341974770886074, -5.184319124889475994, -3.470732244869258132 ) ) ;
#287 = CIRCLE ( 'NONE', #13919, 17.00000000000000000 ) ;
#288 = DIRECTION ( 'NONE',  ( 0.000000000000000000, 0.000000000000000000, -1.000000000000000000 ) ) ;
#289 = APPLICATION_CONTEXT ( 'automotive_design' ) ;
#290 = CARTESIAN_POINT ( 'NONE',  ( -52.77438362644100067, 99.17411849586700612, -145.2984795835770058 ) ) ;
#291 = CARTESIAN_POINT ( 'NONE',  ( -12.81835358098578759, -12.00000029085424202, -0.3335879563140091153 ) ) ;
#292 = EDGE_CURVE ( 'NONE', #3454, #15328, #4849, .T. ) ;
#293 = CIRCLE ( 'NONE', #12448, 3.250000000000016431 ) ;
#294 = ORIENTED_EDGE ( 'NONE', *, *, #12494, .T. ) ;
#295 = DIRECTION ( 'NONE',  ( 1.000000000000000000, 0.000000000000000000, 0.000000000000000000 ) ) ;
#296 = ADVANCED_FACE ( 'NONE', ( #6886 ), #12771, .T. ) ;
#297 = EDGE_LOOP ( 'NONE', ( #2095, #11678 ) ) ;
#298 = MANIFOLD_SOLID_BREP ( 'Cut-Extrude1[3]', #2333 ) ;
#299 = ORIENTED_EDGE ( 'NONE', *, *, #15082, .F. ) ;
#300 = ORIENTED_EDGE ( 'NONE', *, *, #2020, .F. ) ;
#301 = EDGE_LOOP ( 'NONE', ( #12633, #387, #14477, #1085, #12635, #5840, #11093, #4526 ) ) ;
#302 = AXIS2_PLACEMENT_3D ( 'NONE', #4626, #14004, #968 ) ;
#303 = DIRECTION ( 'NONE',  ( -0.000000000000000000, -0.000000000000000000, -1.000000000000000000 ) ) ;
#304 = CARTESIAN_POINT ( 'NONE',  ( -1.090659875871078599, -1.881874999999897824, -3.598793876473114661 ) ) ;
#305 = VECTOR ( 'NONE', #8128, 1000.000000000000000 ) ;
#306 = CARTESIAN_POINT ( 'NONE',  ( 3.389018004338130385, -4.078125000000095035, -1.813062472674689340 ) ) ;
#307 = CARTESIAN_POINT ( 'NONE',  ( 3.637955631634659959, -5.499999999999999112, 4.455210719721457493E-16 ) ) ;
#308 = CYLINDRICAL_SURFACE ( 'NONE', #15272, 4.249999999999996447 ) ;
#309 = CARTESIAN_POINT ( 'NONE',  ( -80.52077156573417938, 60.67411849586702743, -73.34256232478206528 ) ) ;
#310 = CARTESIAN_POINT ( 'NONE',  ( -86.77438362644100778, 96.81621999649657084, -147.9984795835769944 ) ) ;
#311 = CARTESIAN_POINT ( 'NONE',  ( -76.48108760497456160, 68.65632084656354550, -81.84847958357697451 ) ) ;
#312 = AXIS2_PLACEMENT_3D ( 'NONE', #12956, #1156, #3249 ) ;
#313 = ADVANCED_FACE ( 'NONE', ( #6955 ), #3455, .T. ) ;
#314 = CARTESIAN_POINT ( 'NONE',  ( -15.50000000000000000, -0.4000000000000000222, -22.50000000000000000 ) ) ;
#315 = AXIS2_PLACEMENT_3D ( 'NONE', #4207, #7855, #6470 ) ;
#316 = DIRECTION ( 'NONE',  ( -1.000000000000000000, 0.000000000000000000, 0.000000000000000000 ) ) ;
#317 = ORIENTED_EDGE ( 'NONE', *, *, #10977, .T. ) ;
#318 = CARTESIAN_POINT ( 'NONE',  ( -69.77438362644001302, 82.17411849586700612, -93.49847958357699440 ) ) ;
#319 = EDGE_CURVE ( 'NONE', #10983, #14726, #818, .T. ) ;
#320 = ORIENTED_EDGE ( 'NONE', *, *, #1529, .T. ) ;
#321 = AXIS2_PLACEMENT_3D ( 'NONE', #2492, #3670, #13142 ) ;
#322 = EDGE_CURVE ( 'NONE', #15299, #4417, #124, .T. ) ;
#323 = ORIENTED_EDGE ( 'NONE', *, *, #3996, .F. ) ;
#324 = UNCERTAINTY_MEASURE_WITH_UNIT (LENGTH_MEASURE( 1.000000000000000082E-05 ), #9126, 'distance_accuracy_value', 'NONE');
#325 = CARTESIAN_POINT ( 'NONE',  ( -1.792750223658622799, -5.928749999999893383, -2.680858111629535578 ) ) ;
#326 = CARTESIAN_POINT ( 'NONE',  ( -82.27438362643999881, 65.17411849586700612, -86.49847958357699440 ) ) ;
#327 = AXIS2_PLACEMENT_3D ( 'NONE', #4537, #4852, #6031 ) ;
#328 = CARTESIAN_POINT ( 'NONE',  ( 4.251316196654235213, -0.9992135623729603289, -0.001534204912023576835 ) ) ;
#329 = CIRCLE ( 'NONE', #7787, 0.5999999999999999778 ) ;
#330 = MANIFOLD_SOLID_BREP ( 'Cut-Extrude1[2]', #3578 ) ;
#331 = EDGE_CURVE ( 'NONE', #13653, #13217, #4545, .T. ) ;
#332 = CARTESIAN_POINT ( 'NONE',  ( 22.58164641901421632, 11.99999970914576330, -14.13358795631400611 ) ) ;
#333 = DIRECTION ( 'NONE',  ( 0.000000000000000000, 0.000000000000000000, -1.000000000000000000 ) ) ;
#334 = DIRECTION ( 'NONE',  ( 1.000000000000000000, 0.000000000000000000, -6.982962677686266711E-15 ) ) ;
#335 = AXIS2_PLACEMENT_3D ( 'NONE', #8151, #10623, #9451 ) ;
#336 =( BOUNDED_CURVE ( )  B_SPLINE_CURVE ( 3, ( #13396, #4082, #13474, #8809 ),
 .UNSPECIFIED., .F., .F. ) 
 B_SPLINE_CURVE_WITH_KNOTS ( ( 4, 4 ),
 ( 1.570796326794896780, 3.141592653589790896 ),
 .UNSPECIFIED. ) 
 CURVE ( )  GEOMETRIC_REPRESENTATION_ITEM ( )  RATIONAL_B_SPLINE_CURVE ( ( 1.000000000000000000, 0.8047378541243654926, 0.8047378541243654926, 1.000000000000000000 ) ) 
 REPRESENTATION_ITEM ( '' )  );
#337 = DIRECTION ( 'NONE',  ( 0.000000000000000000, 0.000000000000000000, 1.000000000000000000 ) ) ;
#338 = DIRECTION ( 'NONE',  ( -0.000000000000000000, 1.000000000000000000, -0.000000000000000000 ) ) ;
#339 = EDGE_CURVE ( 'NONE', #3097, #10442, #10612, .T. ) ;
#340 = DIRECTION ( 'NONE',  ( -1.000000000000000000, -0.000000000000000000, -0.000000000000000000 ) ) ;
#341 = ORIENTED_EDGE ( 'NONE', *, *, #3984, .F. ) ;
#342 = DIRECTION ( 'NONE',  ( 1.000000000000000000, 0.000000000000000000, 0.000000000000000000 ) ) ;
#343 = AXIS2_PLACEMENT_3D ( 'NONE', #9775, #7400, #13368 ) ;
#344 = VECTOR ( 'NONE', #14343, 1000.000000000000000 ) ;
#345 = EDGE_CURVE ( 'NONE', #11913, #11111, #14089, .T. ) ;
#346 = EDGE_CURVE ( 'NONE', #2409, #13047, #3617, .T. ) ;
#347 = ORIENTED_EDGE ( 'NONE', *, *, #5578, .T. ) ;
#348 =( LENGTH_UNIT ( ) NAMED_UNIT ( * ) SI_UNIT ( .MILLI., .METRE. ) );
#349 = CARTESIAN_POINT ( 'NONE',  ( 2.515861257320511246, -3.140624999999957367, -3.067863912704874796 ) ) ;
#350 = ORIENTED_EDGE ( 'NONE', *, *, #4892, .F. ) ;
#351 = CARTESIAN_POINT ( 'NONE',  ( -0.3627434553294616171, -5.264838562373213904, -3.669149073604559774 ) ) ;
#352 = CARTESIAN_POINT ( 'NONE',  ( 3.852585042300790352, -0.6162500000000914469, -0.7652758215885018256 ) ) ;
#353 = AXIS2_PLACEMENT_3D ( 'NONE', #3405, #4807, #5912 ) ;
#354 = DIRECTION ( 'NONE',  ( -0.9961946980917452121, 7.200509705930738460E-17, -0.08715574274766156593 ) ) ;
#355 = DIRECTION ( 'NONE',  ( 0.000000000000000000, 0.000000000000000000, 1.000000000000000000 ) ) ;
#356 = PLANE ( 'NONE',  #3581 ) ;
#357 = BREP_WITH_VOIDS ( 'NONE', #12735, ( #9878 ) );
#358 = CARTESIAN_POINT ( 'NONE',  ( -69.77438362644001302, 82.17411849586700612, -138.4984795835769944 ) ) ;
#359 = CARTESIAN_POINT ( 'NONE',  ( 0.000000000000000000, 0.000000000000000000, -79.59847958357700293 ) ) ;
#360 = DIRECTION ( 'NONE',  ( -1.000000000000000000, 0.000000000000000000, 0.000000000000000000 ) ) ;
#361 = DIRECTION ( 'NONE',  ( 0.000000000000000000, 0.000000000000000000, -1.000000000000000000 ) ) ;
#362 = PLANE ( 'NONE',  #14403 ) ;
#363 = ORIENTED_EDGE ( 'NONE', *, *, #4204, .F. ) ;
#364 = ORIENTED_EDGE ( 'NONE', *, *, #13152, .F. ) ;
#365 = CARTESIAN_POINT ( 'NONE',  ( 111.1209562785928426, -60.97574601647338000, 151.1287135145406637 ) ) ;
#366 = CONICAL_SURFACE ( 'NONE', #1846, 2.042000000000002036, 1.047197551196596965 ) ;
#367 = ORIENTED_EDGE ( 'NONE', *, *, #5633, .F. ) ;
#368 = CARTESIAN_POINT ( 'NONE',  ( -44.58670980944422269, 0.000000000000000000, 89.50956111919107627 ) ) ;
#369 = CARTESIAN_POINT ( 'NONE',  ( 3.647531283552059467, -2.600625000000050591, -0.3606074429803771131 ) ) ;
#370 = ORIENTED_EDGE ( 'NONE', *, *, #5864, .T. ) ;
#371 = ORIENTED_EDGE ( 'NONE', *, *, #4615, .F. ) ;
#372 = LINE ( 'NONE', #8825, #6733 ) ;
#373 = CARTESIAN_POINT ( 'NONE',  ( 2.801881283053006655, -5.106938005630682120, -2.401640922905785125 ) ) ;
#374 = STYLED_ITEM ( 'NONE', ( #8267 ), #385 ) ;
#375 = DIRECTION ( 'NONE',  ( 1.000000000000000000, 0.000000000000000000, -0.000000000000000000 ) ) ;
#376 = AXIS2_PLACEMENT_3D ( 'NONE', #13204, #2563, #14504 ) ;
#377 = DIRECTION ( 'NONE',  ( 1.000000000000000000, 0.000000000000000000, 0.000000000000000000 ) ) ;
#378 = FACE_BOUND ( 'NONE', #838, .T. ) ;
#379 = VECTOR ( 'NONE', #1869, 1000.000000000000000 ) ;
#380 = CARTESIAN_POINT ( 'NONE',  ( 3.173335668876534399, -5.499999999999995559, 4.202682741317042909E-16 ) ) ;
#381 = FACE_OUTER_BOUND ( 'NONE', #1875, .T. ) ;
#382 = VERTEX_POINT ( 'NONE', #12076 ) ;
#383 = FACE_OUTER_BOUND ( 'NONE', #7346, .T. ) ;
#384 = VERTEX_POINT ( 'NONE', #4938 ) ;
#385 = MANIFOLD_SOLID_BREP ( 'Chamfer1', #11506 ) ;
#386 = ORIENTED_EDGE ( 'NONE', *, *, #13860, .F. ) ;
#387 = ORIENTED_EDGE ( 'NONE', *, *, #8641, .T. ) ;
#388 =( GEOMETRIC_REPRESENTATION_CONTEXT ( 3 ) GLOBAL_UNCERTAINTY_ASSIGNED_CONTEXT ( ( #5155 ) ) GLOBAL_UNIT_ASSIGNED_CONTEXT ( ( #11839, #2746, #8645 ) ) REPRESENTATION_CONTEXT ( 'NONE', 'WORKASPACE' ) );
#389 = VERTEX_POINT ( 'NONE', #5889 ) ;
#390 = VECTOR ( 'NONE', #8485, 1000.000000000000000 ) ;
#391 = DIRECTION ( 'NONE',  ( 0.000000000000000000, -0.000000000000000000, 1.000000000000000000 ) ) ;
#392 = CIRCLE ( 'NONE', #2369, 0.6000000000000000888 ) ;
#393 = EDGE_CURVE ( 'NONE', #14684, #12550, #2354, .T. ) ;
#394 = CARTESIAN_POINT ( 'NONE',  ( -2.084927739720960016, -1.928749999999817888, -3.122072247380865306 ) ) ;
#395 =( NAMED_UNIT ( * ) SI_UNIT ( $, .STERADIAN. ) SOLID_ANGLE_UNIT ( ) );
#396 = CARTESIAN_POINT ( 'NONE',  ( -2.497846391779839248, -3.359374999999932943, -3.045264817802638468 ) ) ;
#397 = FACE_OUTER_BOUND ( 'NONE', #157, .T. ) ;
#398 = EDGE_CURVE ( 'NONE', #12114, #15067, #14313, .T. ) ;
#399 = FACE_OUTER_BOUND ( 'NONE', #13259, .T. ) ;
#400 = DIRECTION ( 'NONE',  ( 9.422394424380278809E-16, -1.000000000000000000, 0.000000000000000000 ) ) ;
#401 = CARTESIAN_POINT ( 'NONE',  ( -52.77438362643999881, 65.17411849586700612, -147.9984795835769944 ) ) ;
#402 = CIRCLE ( 'NONE', #10057, 0.6000000000000000888 ) ;
#403 = CARTESIAN_POINT ( 'NONE',  ( -61.64938362644000591, 82.17411849586700612, -85.04847958357700577 ) ) ;
#404 = CARTESIAN_POINT ( 'NONE',  ( 40.52020888806953991, -24.00000000000000000, 0.000000000000000000 ) ) ;
#405 = CARTESIAN_POINT ( 'NONE',  ( -69.77438362644100778, 92.17411849586700612, -67.49847958357700861 ) ) ;
#406 = CIRCLE ( 'NONE', #9069, 1.999999999999988010 ) ;
#407 = ORIENTED_EDGE ( 'NONE', *, *, #14933, .T. ) ;
#408 = VECTOR ( 'NONE', #14676, 1000.000000000000000 ) ;
#409 = CARTESIAN_POINT ( 'NONE',  ( -52.77438362644100067, 96.81621999649657084, -150.4984795835770228 ) ) ;
#410 = ORIENTED_EDGE ( 'NONE', *, *, #13960, .T. ) ;
#411 = VERTEX_POINT ( 'NONE', #13239 ) ;
#412 = ORIENTED_EDGE ( 'NONE', *, *, #7830, .T. ) ;
#413 = CARTESIAN_POINT ( 'NONE',  ( -2.348309169242666083, -5.210000000000155396, 2.347120911809276400 ) ) ;
#414 = FACE_OUTER_BOUND ( 'NONE', #10961, .T. ) ;
#415 = VECTOR ( 'NONE', #10901, 1000.000000000000000 ) ;
#416 = EDGE_CURVE ( 'NONE', #3919, #9472, #10591, .T. ) ;
#417 = CARTESIAN_POINT ( 'NONE',  ( -2.348309169242665639, -5.210000000000155396, 2.347120911809276400 ) ) ;
#418 = MANIFOLD_SOLID_BREP ( 'Move Face10', #630 ) ;
#419 = FACE_BOUND ( 'NONE', #14484, .T. ) ;
#420 = CARTESIAN_POINT ( 'NONE',  ( -60.52799568714584666, 60.67411849586701322, -152.4984795835769944 ) ) ;
#421 = EDGE_CURVE ( 'NONE', #13943, #13082, #6349, .T. ) ;
#422 = CARTESIAN_POINT ( 'NONE',  ( 68.41329019055577021, 0.000000000000000000, 135.5095611191910621 ) ) ;
#423 = DIRECTION ( 'NONE',  ( 0.000000000000000000, 0.000000000000000000, -1.000000000000000000 ) ) ;
#424 = LINE ( 'NONE', #2671, #3060 ) ;
#425 = DIRECTION ( 'NONE',  ( 0.000000000000000000, 0.000000000000000000, -1.000000000000000000 ) ) ;
#426 = ORIENTED_EDGE ( 'NONE', *, *, #11897, .F. ) ;
#427 = VECTOR ( 'NONE', #13074, 1000.000000000000000 ) ;
#428 = DIRECTION ( 'NONE',  ( 1.000000000000000000, 0.000000000000000000, 0.000000000000000000 ) ) ;
#429 = AXIS2_PLACEMENT_3D ( 'NONE', #8275, #13100, #14013 ) ;
#430 = EDGE_CURVE ( 'NONE', #12493, #12176, #14014, .T. ) ;
#431 = ADVANCED_FACE ( 'NONE', ( #12219 ), #11046, .T. ) ;
#432 = ORIENTED_EDGE ( 'NONE', *, *, #14693, .T. ) ;
#433 =( NAMED_UNIT ( * ) PLANE_ANGLE_UNIT ( ) SI_UNIT ( $, .RADIAN. ) );
#434 = CARTESIAN_POINT ( 'NONE',  ( 3.171456684173084906, -2.109375000000075051, -2.604672169174167884 ) ) ;
#435 = EDGE_LOOP ( 'NONE', ( #14703, #1208, #1894, #9439 ) ) ;
#436 = EDGE_CURVE ( 'NONE', #2455, #11284, #12306, .T. ) ;
#437 = DIRECTION ( 'NONE',  ( 0.000000000000000000, 0.000000000000000000, -1.000000000000000000 ) ) ;
#438 = EDGE_CURVE ( 'NONE', #7835, #506, #1594, .T. ) ;
#439 = LINE ( 'NONE', #12387, #4347 ) ;
#440 = DIRECTION ( 'NONE',  ( 0.000000000000000000, 0.000000000000000000, -1.000000000000000000 ) ) ;
#441 = CARTESIAN_POINT ( 'NONE',  ( 57.41329019055577021, 5.000000000000001776, 125.5408111191910763 ) ) ;
#442 = MANIFOLD_SOLID_BREP ( 'Revolve3', #2613 ) ;
#443 = DIRECTION ( 'NONE',  ( -1.000000000000000000, 0.000000000000000000, 0.000000000000000000 ) ) ;
#444 = CARTESIAN_POINT ( 'NONE',  ( -3.388210470019727971, 7.386374946223608119E-17, -0.2964300057665807953 ) ) ;
#445 = DIRECTION ( 'NONE',  ( 1.287488025362404182E-15, 1.000000000000000000, 0.000000000000000000 ) ) ;
#446 = DIRECTION ( 'NONE',  ( 0.000000000000000000, 0.000000000000000000, 1.000000000000000000 ) ) ;
#447 = DIRECTION ( 'NONE',  ( 0.8660254037844383745, -0.5000000000000003331, 0.000000000000000000 ) ) ;
#448 = EDGE_CURVE ( 'NONE', #11545, #1533, #8802, .T. ) ;
#449 = VERTEX_POINT ( 'NONE', #3990 ) ;
#450 = SHAPE_REPRESENTATION_RELATIONSHIP ( 'NONE' , 'NONE' ,  #4448, #5164 ) ;
#451 = EDGE_LOOP ( 'NONE', ( #11553, #2716, #2919, #8346 ) ) ;
#452 = CIRCLE ( 'NONE', #10103, 1.999999999999988010 ) ;
#453 = DIRECTION ( 'NONE',  ( 0.000000000000000000, 0.000000000000000000, -1.000000000000000000 ) ) ;
#454 = CARTESIAN_POINT ( 'NONE',  ( -3.093239089446946810, -2.178749999999916476, 2.068481483294872358 ) ) ;
#455 = VERTEX_POINT ( 'NONE', #13619 ) ;
#456 = ADVANCED_FACE ( 'NONE', ( #7724 ), #9806, .T. ) ;
#457 = DIRECTION ( 'NONE',  ( 0.000000000000000000, -0.000000000000000000, 1.000000000000000000 ) ) ;
#458 = CARTESIAN_POINT ( 'NONE',  ( -2.941250829588631710, -5.234749468677339479, -1.940783535936075221 ) ) ;
#459 = FACE_OUTER_BOUND ( 'NONE', #3880, .T. ) ;
#460 = VECTOR ( 'NONE', #9602, 1000.000000000000000 ) ;
#461 = CARTESIAN_POINT ( 'NONE',  ( 3.469446951953614189E-15, -24.00000000000000000, 6.000000000000000000 ) ) ;
#462 = DIRECTION ( 'NONE',  ( 1.000000000000000000, 0.000000000000000000, 0.000000000000000000 ) ) ;
#463 = LINE ( 'NONE', #3951, #7338 ) ;
#464 = DIRECTION ( 'NONE',  ( -0.8660254037844387076, -0.4999999999999998890, 0.000000000000000000 ) ) ;
#465 = ORIENTED_EDGE ( 'NONE', *, *, #14188, .T. ) ;
#466 = CARTESIAN_POINT ( 'NONE',  ( 16.25361217826510085, -12.00000029085424025, -0.2147805754215613983 ) ) ;
#467 = VERTEX_POINT ( 'NONE', #2679 ) ;
#468 = ORIENTED_EDGE ( 'NONE', *, *, #7417, .F. ) ;
#469 = VERTEX_POINT ( 'NONE', #11132 ) ;
#470 = ORIENTED_EDGE ( 'NONE', *, *, #7793, .T. ) ;
#471 = EDGE_LOOP ( 'NONE', ( #12338, #12653, #4071, #4133, #10276 ) ) ;
#472 = AXIS2_PLACEMENT_3D ( 'NONE', #3391, #12861, #2220 ) ;
#473 = DIRECTION ( 'NONE',  ( 0.000000000000000000, 1.000000000000000000, 0.000000000000000000 ) ) ;
#474 = CARTESIAN_POINT ( 'NONE',  ( 2.605880849243368491, -2.459999999999848086, 2.603962797083386072 ) ) ;
#475 = PRESENTATION_STYLE_ASSIGNMENT (( #11957 ) ) ;
#476 = CARTESIAN_POINT ( 'NONE',  ( -0.3822054598150002591, -3.734374999999974243, 3.870204888229129114 ) ) ;
#477 = DIRECTION ( 'NONE',  ( -0.000000000000000000, -0.000000000000000000, 1.000000000000000000 ) ) ;
#478 = CYLINDRICAL_SURFACE ( 'NONE', #3382, 4.249999999999996447 ) ;
#479 = DIRECTION ( 'NONE',  ( -0.000000000000000000, -0.000000000000000000, 1.000000000000000000 ) ) ;
#480 = LINE ( 'NONE', #9928, #2075 ) ;
#481 = CARTESIAN_POINT ( 'NONE',  ( -14.25000000000000000, -0.2038245569916330158, 23.22168783648699986 ) ) ;
#482 = CARTESIAN_POINT ( 'NONE',  ( -50.73238362644099197, 100.3530677455522238, -147.9984795835769944 ) ) ;
#483 = DIRECTION ( 'NONE',  ( 1.000000000000000000, 0.000000000000000000, 0.000000000000000000 ) ) ;
#484 = ORIENTED_EDGE ( 'NONE', *, *, #14470, .F. ) ;
#485 = LINE ( 'NONE', #8858, #14927 ) ;
#486 = VERTEX_POINT ( 'NONE', #6013 ) ;
#487 = ORIENTED_EDGE ( 'NONE', *, *, #1261, .T. ) ;
#488 = ORIENTED_EDGE ( 'NONE', *, *, #1646, .T. ) ;
#489 = CARTESIAN_POINT ( 'NONE',  ( -3.090028468548658314, -5.022500000000056808, -1.280849571915205987 ) ) ;
#490 = EDGE_CURVE ( 'NONE', #215, #4608, #7344, .T. ) ;
#491 = DIRECTION ( 'NONE',  ( 0.000000000000000000, 0.000000000000000000, 1.000000000000000000 ) ) ;
#492 = CARTESIAN_POINT ( 'NONE',  ( -3.090028468548657425, -5.022500000000056808, -1.280849571915205765 ) ) ;
#493 = CARTESIAN_POINT ( 'NONE',  ( -80.27438362643999881, 82.17411849586700612, -152.4984795835769944 ) ) ;
#494 = CYLINDRICAL_SURFACE ( 'NONE', #141, 0.6000000000000000888 ) ;
#495 = CARTESIAN_POINT ( 'NONE',  ( -85.77438362644001302, 82.17411849586700612, -93.49847958357699440 ) ) ;
#496 = DIRECTION ( 'NONE',  ( 0.000000000000000000, 1.000000000000000000, 0.000000000000000000 ) ) ;
#497 = DIRECTION ( 'NONE',  ( 0.000000000000000000, 1.000000000000000000, 0.000000000000000000 ) ) ;
#498 = DIRECTION ( 'NONE',  ( -0.000000000000000000, 1.000000000000000000, -0.000000000000000000 ) ) ;
#499 = ORIENTED_EDGE ( 'NONE', *, *, #15094, .T. ) ;
#500 = CARTESIAN_POINT ( 'NONE',  ( 14.25000000000000000, -2.500000000000000000, 23.22168783648699986 ) ) ;
#501 = ADVANCED_FACE ( 'NONE', ( #6177 ), #7170, .F. ) ;
#502 = VERTEX_POINT ( 'NONE', #4752 ) ;
#503 = PRODUCT_DEFINITION_SHAPE ( 'NONE', 'NONE',  #14892 ) ;
#504 = CARTESIAN_POINT ( 'NONE',  ( 17.18164641901421419, -11.40000029085424238, 0.8664120436859875651 ) ) ;
#505 = CARTESIAN_POINT ( 'NONE',  ( -3.121978066431621901, -2.609375000000007550, 2.560763078121147451 ) ) ;
#506 = VERTEX_POINT ( 'NONE', #172 ) ;
#507 = CARTESIAN_POINT ( 'NONE',  ( -77.52077156573416516, 110.1741184958670061, -152.4984795835769944 ) ) ;
#508 = CARTESIAN_POINT ( 'NONE',  ( -62.27438362644000591, 89.17411849586700612, -58.99847958357700151 ) ) ;
#509 = CARTESIAN_POINT ( 'NONE',  ( -69.77438362644001302, 82.17411849586700612, -117.9984795835769944 ) ) ;
#510 = CARTESIAN_POINT ( 'NONE',  ( -52.77438362644000591, 82.17411849586700612, -81.84847958357697451 ) ) ;
#511 = CARTESIAN_POINT ( 'NONE',  ( 0.4577183133098803314, 2.374744442174770764, 4.500000000000000000 ) ) ;
#512 = PLANE ( 'NONE',  #4120 ) ;
#513 = DIRECTION ( 'NONE',  ( 0.9999934663667180423, -1.567696289299852607E-18, 0.003614861529252313879 ) ) ;
#514 = EDGE_CURVE ( 'NONE', #4411, #9101, #13291, .T. ) ;
#515 = CARTESIAN_POINT ( 'NONE',  ( -52.77438362644000591, 65.17411849586700612, -79.59847958357700293 ) ) ;
#516 = ORIENTED_EDGE ( 'NONE', *, *, #4971, .T. ) ;
#517 = EDGE_LOOP ( 'NONE', ( #6569, #13358, #11148, #3402 ) ) ;
#518 = EDGE_CURVE ( 'NONE', #11322, #8008, #639, .T. ) ;
#519 = VECTOR ( 'NONE', #6591, 1000.000000000000000 ) ;
#520 = DIRECTION ( 'NONE',  ( -1.000000000000000000, 0.000000000000000000, 0.000000000000000000 ) ) ;
#521 = EDGE_CURVE ( 'NONE', #12362, #3959, #5064, .T. ) ;
#522 = CARTESIAN_POINT ( 'NONE',  ( -3.566427039428708756, -2.131875000000089670, 1.083295335393480441 ) ) ;
#523 = ORIENTED_EDGE ( 'NONE', *, *, #11573, .T. ) ;
#524 = LINE ( 'NONE', #2855, #12667 ) ;
#525 = AXIS2_PLACEMENT_3D ( 'NONE', #11127, #1437, #6341 ) ;
#526 = EDGE_CURVE ( 'NONE', #897, #10418, #12125, .T. ) ;
#527 = DIRECTION ( 'NONE',  ( 8.034405899049458729E-17, 0.7547095802227716810, -0.6560590289905077199 ) ) ;
#528 = CARTESIAN_POINT ( 'NONE',  ( -15.50000000000000000, -1.037157890325000054, 26.50000000000000000 ) ) ;
#529 = AXIS2_PLACEMENT_3D ( 'NONE', #13605, #6407, #8706 ) ;
#530 = CARTESIAN_POINT ( 'NONE',  ( -86.77438362643999881, 65.17411849586700612, -150.4984795835770228 ) ) ;
#531 = FACE_OUTER_BOUND ( 'NONE', #5335, .T. ) ;
#532 = ADVANCED_FACE ( 'NONE', ( #2423 ), #6094, .F. ) ;
#533 = PLANE ( 'NONE',  #4081 ) ;
#534 = ORIENTED_EDGE ( 'NONE', *, *, #859, .T. ) ;
#535 = DIRECTION ( 'NONE',  ( 0.000000000000000000, 0.000000000000000000, 1.000000000000000000 ) ) ;
#536 = ORIENTED_EDGE ( 'NONE', *, *, #7075, .T. ) ;
#537 = VECTOR ( 'NONE', #14076, 1000.000000000000000 ) ;
#538 = EDGE_LOOP ( 'NONE', ( #9721, #11855, #10440, #988 ) ) ;
#539 = ORIENTED_EDGE ( 'NONE', *, *, #8974, .T. ) ;
#540 = ORIENTED_EDGE ( 'NONE', *, *, #2131, .F. ) ;
#541 = VERTEX_POINT ( 'NONE', #8623 ) ;
#542 = CARTESIAN_POINT ( 'NONE',  ( -59.02799568714584666, 0.000000000000000000, -152.4984795835769944 ) ) ;
#543 = AXIS2_PLACEMENT_3D ( 'NONE', #12547, #5252, #11219 ) ;
#544 = FACE_OUTER_BOUND ( 'NONE', #4192, .T. ) ;
#545 = CARTESIAN_POINT ( 'NONE',  ( -1.508667427112231785, -3.312499999999990674, -3.644952880303303555 ) ) ;
#546 = CARTESIAN_POINT ( 'NONE',  ( -104.2743836264399988, 111.1741184958670061, -79.49847958357700861 ) ) ;
#547 = CARTESIAN_POINT ( 'NONE',  ( -61.59970400812709102, 70.01464610989972925, -81.84847958357697451 ) ) ;
#548 = AXIS2_PLACEMENT_3D ( 'NONE', #9377, #14114, #15187 ) ;
#549 = CARTESIAN_POINT ( 'NONE',  ( -3.440513747128907784, 2.288586792248386903, -3.040855385833559854 ) ) ;
#550 = CARTESIAN_POINT ( 'NONE',  ( -4.010754789764311212, -1.453125000000109912, -1.215065766439024975 ) ) ;
#551 = CARTESIAN_POINT ( 'NONE',  ( -5.196152422706630247, 0.1227504548087275521, -7.569115911492098221E-16 ) ) ;
#552 = CARTESIAN_POINT ( 'NONE',  ( -14.25000000000000000, -2.500000000000000000, 23.22168783648699986 ) ) ;
#553 = CARTESIAN_POINT ( 'NONE',  ( -15.50000000000000000, -1.037157890325000054, -19.00000000000000000 ) ) ;
#554 = EDGE_LOOP ( 'NONE', ( #14518, #4651, #12673, #5642 ) ) ;
#555 = AXIS2_PLACEMENT_3D ( 'NONE', #5570, #7949, #4702 ) ;
#556 = EDGE_LOOP ( 'NONE', ( #3420, #4653, #2541, #2426, #5631, #2495, #10644, #3786 ) ) ;
#557 = VERTEX_POINT ( 'NONE', #10954 ) ;
#558 = VERTEX_POINT ( 'NONE', #4985 ) ;
#559 = CIRCLE ( 'NONE', #10455, 0.5999999999999998668 ) ;
#560 = DIRECTION ( 'NONE',  ( -1.000000000000000000, 0.000000000000000000, 0.000000000000000000 ) ) ;
#561 = CARTESIAN_POINT ( 'NONE',  ( -77.89938362643999881, 82.17411849586700612, -85.04847958357699156 ) ) ;
#562 = CARTESIAN_POINT ( 'NONE',  ( 15.50000000000000000, -1.037157890325000054, -26.50000000000000000 ) ) ;
#563 = PLANE ( 'NONE',  #11832 ) ;
#564 = CARTESIAN_POINT ( 'NONE',  ( -2.598582712860348032, -0.4995676945082659359, 3.267044563363100895 ) ) ;
#565 = ADVANCED_FACE ( 'NONE', ( #9777 ), #14512, .F. ) ;
#566 = VECTOR ( 'NONE', #14294, 1000.000000000000000 ) ;
#567 = CARTESIAN_POINT ( 'NONE',  ( -3.336666538900096679, -5.084999999999988418, 0.001247370357366475637 ) ) ;
#568 = ORIENTED_EDGE ( 'NONE', *, *, #10428, .F. ) ;
#569 = LINE ( 'NONE', #5318, #8356 ) ;
#570 = ORIENTED_EDGE ( 'NONE', *, *, #1954, .T. ) ;
#571 = AXIS2_PLACEMENT_3D ( 'NONE', #14495, #9610, #8611 ) ;
#572 = CARTESIAN_POINT ( 'NONE',  ( -3.978302601493375334, -2.468750000000105693, -0.7924256976418916354 ) ) ;
#573 = EDGE_LOOP ( 'NONE', ( #4904, #6585 ) ) ;
#574 = AXIS2_PLACEMENT_3D ( 'NONE', #12587, #10085, #7779 ) ;
#575 = DIRECTION ( 'NONE',  ( -1.000000000000000000, 0.000000000000000000, 0.000000000000000000 ) ) ;
#576 = EDGE_CURVE ( 'NONE', #1167, #13856, #4919, .T. ) ;
#577 = DIRECTION ( 'NONE',  ( 1.000000000000000000, 0.000000000000000000, 0.000000000000000000 ) ) ;
#578 = CARTESIAN_POINT ( 'NONE',  ( -75.01311196519617397, 67.29799558322736175, -81.84847958357697451 ) ) ;
#579 = CIRCLE ( 'NONE', #11243, 1.449999999999996403 ) ;
#580 = EDGE_CURVE ( 'NONE', #13163, #4486, #254, .T. ) ;
#581 = CIRCLE ( 'NONE', #80, 3.499999999999999556 ) ;
#582 = LINE ( 'NONE', #13561, #8644 ) ;
#583 = LINE ( 'NONE', #14698, #1556 ) ;
#584 = DIRECTION ( 'NONE',  ( 0.000000000000000000, 0.000000000000000000, -1.000000000000000000 ) ) ;
#585 = FACE_OUTER_BOUND ( 'NONE', #1025, .T. ) ;
#586 = CARTESIAN_POINT ( 'NONE',  ( 0.000000000000000000, 0.000000000000000000, 6.000000000000000000 ) ) ;
#587 = VERTEX_POINT ( 'NONE', #3898 ) ;
#588 = ORIENTED_EDGE ( 'NONE', *, *, #11348, .F. ) ;
#589 = DIRECTION ( 'NONE',  ( 0.000000000000000000, 0.5000000000000199840, 0.8660254037844271613 ) ) ;
#590 = CARTESIAN_POINT ( 'NONE',  ( -2.084927739720960460, -1.928749999999817888, -3.122072247380865306 ) ) ;
#591 = ORIENTED_EDGE ( 'NONE', *, *, #448, .T. ) ;
#592 = AXIS2_PLACEMENT_3D ( 'NONE', #8213, #2313, #12876 ) ;
#593 = AXIS2_PLACEMENT_3D ( 'NONE', #5582, #6516, #11379 ) ;
#594 = CARTESIAN_POINT ( 'NONE',  ( 15.50000000000000000, -5.000000000000000000, -19.00000000000000000 ) ) ;
#595 = EDGE_CURVE ( 'NONE', #13129, #8137, #10804, .T. ) ;
#596 = DIRECTION ( 'NONE',  ( -1.000000000000000000, 0.000000000000000000, 0.000000000000000000 ) ) ;
#597 = CARTESIAN_POINT ( 'NONE',  ( 3.464101615137753054, 8.706078090612013285E-15, -3.000000000000000444 ) ) ;
#598 = EDGE_CURVE ( 'NONE', #7295, #15255, #3873, .T. ) ;
#599 = DIRECTION ( 'NONE',  ( 0.000000000000000000, 1.000000000000000000, 0.000000000000000000 ) ) ;
#600 =( LENGTH_UNIT ( ) NAMED_UNIT ( * ) SI_UNIT ( .MILLI., .METRE. ) );
#601 = DIRECTION ( 'NONE',  ( 0.000000000000000000, 0.000000000000000000, -1.000000000000000000 ) ) ;
#602 = AXIS2_PLACEMENT_3D ( 'NONE', #3092, #14863, #1848 ) ;
#603 = DIRECTION ( 'NONE',  ( 0.000000000000000000, 0.000000000000000000, 1.000000000000000000 ) ) ;
#604 = ORIENTED_EDGE ( 'NONE', *, *, #11290, .F. ) ;
#605 = FACE_OUTER_BOUND ( 'NONE', #1148, .T. ) ;
#606 = ORIENTED_EDGE ( 'NONE', *, *, #7544, .T. ) ;
#607 = EDGE_CURVE ( 'NONE', #1588, #4413, #13538, .T. ) ;
#608 = ORIENTED_EDGE ( 'NONE', *, *, #10263, .T. ) ;
#609 = ORIENTED_EDGE ( 'NONE', *, *, #6334, .F. ) ;
#610 = EDGE_CURVE ( 'NONE', #3634, #11545, #14210, .T. ) ;
#611 = ORIENTED_EDGE ( 'NONE', *, *, #11056, .T. ) ;
#612 = ORIENTED_EDGE ( 'NONE', *, *, #8854, .F. ) ;
#613 = CARTESIAN_POINT ( 'NONE',  ( 3.589928677163299220, -5.999213562373140185, 0.0009248216214229900388 ) ) ;
#614 = CARTESIAN_POINT ( 'NONE',  ( -2.355664480073890399, -2.225624999999979092, 2.872538697791624518 ) ) ;
#615 = EDGE_CURVE ( 'NONE', #7422, #10445, #10046, .T. ) ;
#616 = AXIS2_PLACEMENT_3D ( 'NONE', #13381, #1660, #8559 ) ;
#617 = CARTESIAN_POINT ( 'NONE',  ( 1.826535687659961660, -3.828124999999970246, 3.419360526609917628 ) ) ;
#618 = CARTESIAN_POINT ( 'NONE',  ( 14.25000000000000000, -0.2038245569916330158, -21.77831216351300014 ) ) ;
#619 = CARTESIAN_POINT ( 'NONE',  ( -52.77438362644000591, 65.17411849586700612, -86.49847958357699440 ) ) ;
#620 = EDGE_CURVE ( 'NONE', #9201, #8717, #3737, .T. ) ;
#621 = ADVANCED_FACE ( 'NONE', ( #4203 ), #625, .F. ) ;
#622 = CARTESIAN_POINT ( 'NONE',  ( -61.59970400812709102, 70.01464610989972925, -83.44847958357698303 ) ) ;
#623 = CARTESIAN_POINT ( 'NONE',  ( -1.612261674935887568, -1.312500000000171863, -3.888369303904286589 ) ) ;
#624 = DIRECTION ( 'NONE',  ( 1.000000000000000000, 0.000000000000000000, 0.000000000000000000 ) ) ;
#625 = PLANE ( 'NONE',  #12545 ) ;
#626 = PRODUCT_DEFINITION_SHAPE ( 'NONE', 'NONE',  #15168 ) ;
#627 = CARTESIAN_POINT ( 'NONE',  ( -15.50000000000000000, -0.2038245569916614930, -21.05662432702600029 ) ) ;
#628 = ORIENTED_EDGE ( 'NONE', *, *, #8187, .F. ) ;
#629 = MECHANICAL_DESIGN_GEOMETRIC_PRESENTATION_REPRESENTATION (  '', ( #3103 ), #2611 ) ;
#630 = CLOSED_SHELL ( 'NONE', ( #9474, #9132, #12966, #1902, #8555, #15074, #6488, #13690, #5762, #8386, #1849, #1749, #1679, #13727 ) ) ;
#631 = ORIENTED_EDGE ( 'NONE', *, *, #5639, .T. ) ;
#632 = VERTEX_POINT ( 'NONE', #10151 ) ;
#633 = ORIENTED_EDGE ( 'NONE', *, *, #10187, .T. ) ;
#634 = VECTOR ( 'NONE', #10290, 1000.000000000000000 ) ;
#635 = PRODUCT_DEFINITION_CONTEXT ( 'detailed design', #8332, 'design' ) ;
#636 = LINE ( 'NONE', #326, #1022 ) ;
#637 = CARTESIAN_POINT ( 'NONE',  ( -2.589953986283601850, -4.975625000000236220, -2.126619835350766152 ) ) ;
#638 = CARTESIAN_POINT ( 'NONE',  ( -62.02799568714584666, 0.000000000000000000, -152.4984795835769944 ) ) ;
#639 = CIRCLE ( 'NONE', #15241, 4.362044368365340041 ) ;
#640 = PLANE ( 'NONE',  #6024 ) ;
#641 = CARTESIAN_POINT ( 'NONE',  ( -3.031088913245534311, 0.04639863247562460435, -3.750000000000000444 ) ) ;
#642 = AXIS2_PLACEMENT_3D ( 'NONE', #2822, #11192, #3981 ) ;
#643 = DIRECTION ( 'NONE',  ( 0.000000000000000000, 0.000000000000000000, -1.000000000000000000 ) ) ;
#644 = FACE_OUTER_BOUND ( 'NONE', #5137, .T. ) ;
#645 = AXIS2_PLACEMENT_3D ( 'NONE', #14851, #1827, #14781 ) ;
#646 = B_SPLINE_CURVE_WITH_KNOTS ( 'NONE', 3,
 ( #7069, #3331, #8063, #12799, #4573, #9298, #8145, #6150, #8215, #13039, #13186, #2316 ),
 .UNSPECIFIED., .F., .F.,
 ( 4, 2, 2, 2, 2, 4 ),
 ( 2.544323688695373385E-07, 0.001342108318545691186, 0.002013035261634102662, 0.002683962204722513054, 0.004025816090899333836, 0.005367669977076155487 ),
 .UNSPECIFIED. ) ;
#647 = DIRECTION ( 'NONE',  ( -0.8660254037844485886, 0.000000000000000000, -0.4999999999999827360 ) ) ;
#648 = ORIENTED_EDGE ( 'NONE', *, *, #2337, .F. ) ;
#649 = CARTESIAN_POINT ( 'NONE',  ( 15.50000000000000000, -0.2000000000000000111, 25.80000000297970075 ) ) ;
#650 = ORIENTED_EDGE ( 'NONE', *, *, #14893, .F. ) ;
#651 = AXIS2_PLACEMENT_3D ( 'NONE', #6543, #2963, #12274 ) ;
#652 = ORIENTED_EDGE ( 'NONE', *, *, #1449, .F. ) ;
#653 = AXIS2_PLACEMENT_3D ( 'NONE', #7648, #14451, #14528 ) ;
#654 = CARTESIAN_POINT ( 'NONE',  ( 2.924917369268297485, -1.874999999999847455, 2.922799279172734632 ) ) ;
#655 = EDGE_LOOP ( 'NONE', ( #1300, #8723, #4606, #8416 ) ) ;
#656 = AXIS2_PLACEMENT_3D ( 'NONE', #9390, #1174, #6005 ) ;
#657 = FACE_OUTER_BOUND ( 'NONE', #8173, .T. ) ;
#658 = DIRECTION ( 'NONE',  ( 8.034405899049458729E-17, 0.7547095802227716810, -0.6560590289905077199 ) ) ;
#659 = LINE ( 'NONE', #5414, #2818 ) ;
#660 = CIRCLE ( 'NONE', #12071, 3.499999999999999556 ) ;
#661 = CONICAL_SURFACE ( 'NONE', #10574, 3.750000000000003553, 0.7853981633974476129 ) ;
#662 = DIRECTION ( 'NONE',  ( 0.000000000000000000, 0.000000000000000000, 1.000000000000000000 ) ) ;
#663 = CARTESIAN_POINT ( 'NONE',  ( -1.120937138200071015, 2.242130364950076782, 4.499999999999999112 ) ) ;
#664 = CARTESIAN_POINT ( 'NONE',  ( -2.598076211353315568, 0.1227504548087345604, 4.500000000000000888 ) ) ;
#665 = CARTESIAN_POINT ( 'NONE',  ( -67.55245199152457758, 98.02101855758749593, -94.16081083965335097 ) ) ;
#666 = CARTESIAN_POINT ( 'NONE',  ( 21.98164641901421135, -11.40000029085424238, -0.3335879563140091153 ) ) ;
#667 = EDGE_CURVE ( 'NONE', #10367, #5341, #9792, .T. ) ;
#668 = ORIENTED_EDGE ( 'NONE', *, *, #12451, .T. ) ;
#669 = CARTESIAN_POINT ( 'NONE',  ( 17.10018810948620072, -11.27427741823326279, 0.2691656137646578073 ) ) ;
#670 = CARTESIAN_POINT ( 'NONE',  ( -3.204583014436231281, -1.178749999999988640, 2.140022251743640691 ) ) ;
#671 = ORIENTED_EDGE ( 'NONE', *, *, #799, .F. ) ;
#672 = AXIS2_PLACEMENT_3D ( 'NONE', #12988, #15, #10403 ) ;
#673 = EDGE_CURVE ( 'NONE', #10438, #8132, #3367, .T. ) ;
#674 = CIRCLE ( 'NONE', #1917, 4.000000000000000000 ) ;
#675 = CARTESIAN_POINT ( 'NONE',  ( -61.72438362644000165, 82.17411849586700612, -80.44847958357698303 ) ) ;
#676 = LINE ( 'NONE', #4328, #6394 ) ;
#677 = CARTESIAN_POINT ( 'NONE',  ( -69.77438362644100778, 72.17411849586700612, -79.49847958357700861 ) ) ;
#678 = DIRECTION ( 'NONE',  ( -1.000000000000000000, 0.000000000000000000, 0.000000000000000000 ) ) ;
#679 = CARTESIAN_POINT ( 'NONE',  ( 15.50000000000000000, -2.500000000000000000, -21.05662432702600029 ) ) ;
#680 = CARTESIAN_POINT ( 'NONE',  ( 14.25000000000000000, -2.500000000000000000, -21.77831216351300014 ) ) ;
#681 = LINE ( 'NONE', #5433, #14902 ) ;
#682 = VERTEX_POINT ( 'NONE', #13445 ) ;
#683 = DIRECTION ( 'NONE',  ( 0.000000000000000000, 0.000000000000000000, -1.000000000000000000 ) ) ;
#684 = ADVANCED_FACE ( 'NONE', ( #11177 ), #13521, .F. ) ;
#685 = ORIENTED_EDGE ( 'NONE', *, *, #9338, .T. ) ;
#686 = VERTEX_POINT ( 'NONE', #3114 ) ;
#687 = EDGE_LOOP ( 'NONE', ( #7655, #1654 ) ) ;
#688 = ORIENTED_EDGE ( 'NONE', *, *, #13426, .F. ) ;
#689 = EDGE_CURVE ( 'NONE', #13826, #3095, #14258, .T. ) ;
#690 = ORIENTED_EDGE ( 'NONE', *, *, #12073, .F. ) ;
#691 = CARTESIAN_POINT ( 'NONE',  ( -0.001316410337383604624, -6.249213562373078013, -3.556817731968370033 ) ) ;
#692 = CARTESIAN_POINT ( 'NONE',  ( -0.3768771888557862493, -1.319375000000004405, 3.816279424444235069 ) ) ;
#693 = AXIS2_PLACEMENT_3D ( 'NONE', #11712, #11636, #14039 ) ;
#694 = DIRECTION ( 'NONE',  ( -1.000000000000000000, 0.000000000000000000, 0.000000000000000000 ) ) ;
#695 = CARTESIAN_POINT ( 'NONE',  ( 2.924917369268297485, -1.874999999999847455, 2.922799279172734632 ) ) ;
#696 = DIRECTION ( 'NONE',  ( -9.422394424380278809E-16, 1.000000000000000000, -0.000000000000000000 ) ) ;
#697 = CARTESIAN_POINT ( 'NONE',  ( 10.10406781373725771, 10.99999970914572778, 69.08979243323354069 ) ) ;
#698 = EDGE_CURVE ( 'NONE', #4969, #8760, #13664, .T. ) ;
#699 = CARTESIAN_POINT ( 'NONE',  ( -5.196152422706634688, 1.678847577293359539, -8.911270275552416508E-16 ) ) ;
#700 = CARTESIAN_POINT ( 'NONE',  ( -3.324804228637022074, -0.6093749999999287237, 2.730601746129839746 ) ) ;
#701 = CARTESIAN_POINT ( 'NONE',  ( -84.73238362643999722, 63.99516924618178848, -150.4984795835770228 ) ) ;
#702 = DIRECTION ( 'NONE',  ( -2.551930889570659960E-15, 1.000000000000000000, 0.000000000000000000 ) ) ;
#703 = CARTESIAN_POINT ( 'NONE',  ( -15.91434062215688350, -0.3156604612129211285, -21.29584399676446793 ) ) ;
#704 = VERTEX_POINT ( 'NONE', #10084 ) ;
#705 = DIRECTION ( 'NONE',  ( -1.000000000000000000, 0.000000000000000000, 0.000000000000000000 ) ) ;
#706 = EDGE_CURVE ( 'NONE', #9229, #2624, #7635, .T. ) ;
#707 = ORIENTED_EDGE ( 'NONE', *, *, #4, .F. ) ;
#708 = AXIS2_PLACEMENT_3D ( 'NONE', #11617, #5583, #12482 ) ;
#709 = ORIENTED_EDGE ( 'NONE', *, *, #610, .T. ) ;
#710 = ORIENTED_EDGE ( 'NONE', *, *, #7264, .F. ) ;
#711 = ADVANCED_FACE ( 'NONE', ( #14882 ), #12425, .F. ) ;
#712 = DIRECTION ( 'NONE',  ( 0.9961946980917452121, -7.200509705930739692E-17, 0.08715574274766157981 ) ) ;
#713 = EDGE_CURVE ( 'NONE', #10232, #13570, #9817, .T. ) ;
#714 = CARTESIAN_POINT ( 'NONE',  ( -0.6461339251375918247, -5.303750000000252207, 3.244047683681893446 ) ) ;
#715 = FACE_BOUND ( 'NONE', #7426, .T. ) ;
#716 = DIRECTION ( 'NONE',  ( 0.000000000000000000, 0.000000000000000000, 1.000000000000000000 ) ) ;
#717 = DIRECTION ( 'NONE',  ( 1.000000000000000000, 0.000000000000000000, 0.000000000000000000 ) ) ;
#718 = CIRCLE ( 'NONE', #14335, 8.124999999999992895 ) ;
#719 = LINE ( 'NONE', #4067, #9840 ) ;
#720 = CARTESIAN_POINT ( 'NONE',  ( -2.226241924188425703, -0.4995676945082649367, 3.513072387502060412 ) ) ;
#721 = CARTESIAN_POINT ( 'NONE',  ( -52.77438362643999881, 65.17411849586700612, -150.4984795835770228 ) ) ;
#722 = DIRECTION ( 'NONE',  ( -1.000000000000000000, 0.000000000000000000, 0.000000000000000000 ) ) ;
#723 = ORIENTED_EDGE ( 'NONE', *, *, #792, .F. ) ;
#724 = FACE_OUTER_BOUND ( 'NONE', #247, .T. ) ;
#725 = EDGE_CURVE ( 'NONE', #13232, #1792, #6398, .T. ) ;
#726 = VERTEX_POINT ( 'NONE', #404 ) ;
#727 = FACE_OUTER_BOUND ( 'NONE', #7858, .T. ) ;
#728 = ORIENTED_EDGE ( 'NONE', *, *, #5464, .T. ) ;
#729 = CARTESIAN_POINT ( 'NONE',  ( -1.243836315904764955, -0.7031249999999807931, 4.105705763534058583 ) ) ;
#730 = ORIENTED_EDGE ( 'NONE', *, *, #6098, .F. ) ;
#731 = CARTESIAN_POINT ( 'NONE',  ( -3.614955235551140511, -3.561713562373173936, 1.496253015928757701 ) ) ;
#732 = DIRECTION ( 'NONE',  ( -0.000000000000000000, 1.000000000000000000, -0.000000000000000000 ) ) ;
#733 = DIRECTION ( 'NONE',  ( 0.000000000000000000, 0.000000000000000000, 1.000000000000000000 ) ) ;
#734 = LINE ( 'NONE', #962, #11977 ) ;
#735 = DIRECTION ( 'NONE',  ( -1.000000000000000000, 0.000000000000000000, 0.000000000000000000 ) ) ;
#736 = FACE_OUTER_BOUND ( 'NONE', #12730, .T. ) ;
#737 = LINE ( 'NONE', #11142, #6125 ) ;
#738 = CARTESIAN_POINT ( 'NONE',  ( -69.77438362644001302, 82.17411849586700612, -150.4984795835769944 ) ) ;
#739 = DIRECTION ( 'NONE',  ( 0.000000000000000000, 0.000000000000000000, 1.000000000000000000 ) ) ;
#740 = ORIENTED_EDGE ( 'NONE', *, *, #6624, .F. ) ;
#741 = CARTESIAN_POINT ( 'NONE',  ( -2.629016928070554204, -2.210000000000078568, 2.627652665972901147 ) ) ;
#742 = ORIENTED_EDGE ( 'NONE', *, *, #277, .F. ) ;
#743 = CARTESIAN_POINT ( 'NONE',  ( -91.27438362643999881, 65.17411849586700612, -86.49847958357699440 ) ) ;
#744 = CARTESIAN_POINT ( 'NONE',  ( -59.02799568714584666, 164.3482369917340122, -152.4984795835769944 ) ) ;
#745 = DIRECTION ( 'NONE',  ( 0.000000000000000000, 1.000000000000000000, 0.000000000000000000 ) ) ;
#746 = DIRECTION ( 'NONE',  ( 0.000000000000000000, 4.336808689942017736E-16, -1.000000000000000000 ) ) ;
#747 = CARTESIAN_POINT ( 'NONE',  ( 15.50000000000000000, -1.037157890325000054, 22.50000000000000000 ) ) ;
#748 = EDGE_CURVE ( 'NONE', #59, #4906, #2885, .T. ) ;
#749 = DIRECTION ( 'NONE',  ( 0.000000000000000000, 0.000000000000000000, -1.000000000000000000 ) ) ;
#750 = ORIENTED_EDGE ( 'NONE', *, *, #7341, .T. ) ;
#751 = CARTESIAN_POINT ( 'NONE',  ( -50.02438362644000591, 65.17411849586700612, -152.4984795835769944 ) ) ;
#752 = ORIENTED_EDGE ( 'NONE', *, *, #11402, .T. ) ;
#753 = ORIENTED_EDGE ( 'NONE', *, *, #1823, .T. ) ;
#754 = CARTESIAN_POINT ( 'NONE',  ( -1.562933739280453427, -5.256875000000181153, 2.922265072135110664 ) ) ;
#755 = ORIENTED_EDGE ( 'NONE', *, *, #5452, .T. ) ;
#756 = ORIENTED_EDGE ( 'NONE', *, *, #1230, .F. ) ;
#757 = ORIENTED_EDGE ( 'NONE', *, *, #10286, .F. ) ;
#758 = AXIS2_PLACEMENT_3D ( 'NONE', #7496, #7418, #6415 ) ;
#759 = DIRECTION ( 'NONE',  ( 1.000000000000000000, 0.000000000000000000, 0.000000000000000000 ) ) ;
#760 = CARTESIAN_POINT ( 'NONE',  ( 1.112125432426118499, -1.381875000000161391, 3.661359949639011901 ) ) ;
#761 = DIRECTION ( 'NONE',  ( 0.000000000000000000, 1.000000000000000000, 0.000000000000000000 ) ) ;
#762 = CARTESIAN_POINT ( 'NONE',  ( 3.171456684173084906, -2.109375000000075051, -2.604672169174167884 ) ) ;
#763 = CARTESIAN_POINT ( 'NONE',  ( -35.58670980944424400, 5.000000000000000000, 131.2954986191910791 ) ) ;
#764 = EDGE_CURVE ( 'NONE', #13867, #7621, #14028, .T. ) ;
#765 = CARTESIAN_POINT ( 'NONE',  ( 57.41329019055577021, 5.000000000000000000, 95.72362361919107343 ) ) ;
#766 = CARTESIAN_POINT ( 'NONE',  ( 35.35543536254876074, -3.618985300545107364, 6.000000000000000000 ) ) ;
#767 = CARTESIAN_POINT ( 'NONE',  ( 1.916065064279496746E-15, 7.362499999999997158, 0.000000000000000000 ) ) ;
#768 = LINE ( 'NONE', #1789, #12528 ) ;
#769 = EDGE_CURVE ( 'NONE', #2388, #13148, #7355, .T. ) ;
#770 = CARTESIAN_POINT ( 'NONE',  ( 16.75000000000000000, -0.2714405302574886547, 22.01253933645462624 ) ) ;
#771 = AXIS2_PLACEMENT_3D ( 'NONE', #6411, #4147, #2977 ) ;
#772 = ORIENTED_EDGE ( 'NONE', *, *, #3947, .T. ) ;
#773 = DIRECTION ( 'NONE',  ( 0.8660254037844387076, 0.4999999999999998890, 0.000000000000000000 ) ) ;
#774 = ORIENTED_EDGE ( 'NONE', *, *, #232, .T. ) ;
#775 = AXIS2_PLACEMENT_3D ( 'NONE', #10023, #10964, #5075 ) ;
#776 = ORIENTED_EDGE ( 'NONE', *, *, #5824, .T. ) ;
#777 = VERTEX_POINT ( 'NONE', #6467 ) ;
#778 = PRODUCT_DEFINITION_CONTEXT ( 'detailed design', #1975, 'design' ) ;
#779 = AXIS2_PLACEMENT_3D ( 'NONE', #13782, #9894, #12321 ) ;
#780 = LINE ( 'NONE', #4511, #9954 ) ;
#781 = CARTESIAN_POINT ( 'NONE',  ( 0.001278483876788636883, -4.335000000000164277, 3.435880605283331501 ) ) ;
#782 = AXIS2_PLACEMENT_3D ( 'NONE', #3127, #7999, #7863 ) ;
#783 = FACE_OUTER_BOUND ( 'NONE', #4137, .T. ) ;
#784 = CARTESIAN_POINT ( 'NONE',  ( -86.77438362644001302, 99.17411849586700612, -79.59847958357700293 ) ) ;
#785 = ADVANCED_FACE ( 'NONE', ( #13597 ), #11109, .F. ) ;
#786 = LINE ( 'NONE', #13977, #3884 ) ;
#787 = AXIS2_PLACEMENT_3D ( 'NONE', #14350, #6082, #2412 ) ;
#788 = DIRECTION ( 'NONE',  ( 0.8660254037844381525, 1.060575238724905436E-16, -0.5000000000000007772 ) ) ;
#789 = DIRECTION ( 'NONE',  ( 0.000000000000000000, 0.000000000000000000, -1.000000000000000000 ) ) ;
#790 = CARTESIAN_POINT ( 'NONE',  ( -91.27438362643999881, 99.17411849586700612, -145.4984795835769660 ) ) ;
#791 = AXIS2_PLACEMENT_3D ( 'NONE', #4393, #3219, #6883 ) ;
#792 = EDGE_CURVE ( 'NONE', #7940, #3694, #4366, .T. ) ;
#793 = ORIENTED_EDGE ( 'NONE', *, *, #9979, .T. ) ;
#794 = DIRECTION ( 'NONE',  ( -0.000000000000000000, 1.000000000000000000, -0.000000000000000000 ) ) ;
#795 = EDGE_LOOP ( 'NONE', ( #11221, #317, #14436, #2392, #10585 ) ) ;
#796 = STYLED_ITEM ( 'NONE', ( #8444 ), #10531 ) ;
#797 = LINE ( 'NONE', #13911, #5495 ) ;
#798 = ORIENTED_EDGE ( 'NONE', *, *, #12472, .T. ) ;
#799 = EDGE_CURVE ( 'NONE', #1408, #5494, #8855, .T. ) ;
#800 = CARTESIAN_POINT ( 'NONE',  ( -4.293856390582560856, -0.5156249999999756861, 0.4244695705039617240 ) ) ;
#801 = ORIENTED_EDGE ( 'NONE', *, *, #3085, .T. ) ;
#802 = CIRCLE ( 'NONE', #3288, 4.499999999999997335 ) ;
#803 = CARTESIAN_POINT ( 'NONE',  ( -4.035363762266634957, -2.483588562372986086, -0.3985244866878402958 ) ) ;
#804 = DIRECTION ( 'NONE',  ( 1.747085166004344019E-15, -1.000000000000000000, 0.000000000000000000 ) ) ;
#805 = EDGE_CURVE ( 'NONE', #71, #7389, #9667, .T. ) ;
#806 = DIRECTION ( 'NONE',  ( -1.000000000000000000, 0.000000000000000000, 0.000000000000000000 ) ) ;
#807 = VECTOR ( 'NONE', #13371, 1000.000000000000000 ) ;
#808 = FACE_OUTER_BOUND ( 'NONE', #14949, .T. ) ;
#809 = ADVANCED_FACE ( 'NONE', ( #11486 ), #4663, .T. ) ;
#810 = CARTESIAN_POINT ( 'NONE',  ( 21.98164641901421135, -12.50000029085423847, -8.775548064764199907 ) ) ;
#811 = EDGE_CURVE ( 'NONE', #11511, #3473, #14043, .T. ) ;
#812 = DIRECTION ( 'NONE',  ( -1.000000000000000000, 0.000000000000000000, 0.000000000000000000 ) ) ;
#813 = AXIS2_PLACEMENT_3D ( 'NONE', #12268, #1639, #8994 ) ;
#814 = CIRCLE ( 'NONE', #8252, 4.709525205202999665 ) ;
#815 = CARTESIAN_POINT ( 'NONE',  ( -66.41143315690761995, 66.60412428008086749, -83.44847958357698303 ) ) ;
#816 = CARTESIAN_POINT ( 'NONE',  ( 74.62798945165403097, 22.84757080772592275, 62.32699674934021061 ) ) ;
#817 = ORIENTED_EDGE ( 'NONE', *, *, #6878, .F. ) ;
#818 = LINE ( 'NONE', #5573, #3352 ) ;
#819 = CARTESIAN_POINT ( 'NONE',  ( 2.349903878712679806, -5.140624999999672262, -2.861852458627701434 ) ) ;
#820 = ORIENTED_EDGE ( 'NONE', *, *, #1709, .T. ) ;
#821 = CARTESIAN_POINT ( 'NONE',  ( 2.100337907687909400, -1.741249999999995968, -3.141606438102765075 ) ) ;
#822 = AXIS2_PLACEMENT_3D ( 'NONE', #12682, #4233, #2055 ) ;
#823 = CARTESIAN_POINT ( 'NONE',  ( -16.94999999999999929, -0.2000000000000000111, -22.50000000000000000 ) ) ;
#824 = VECTOR ( 'NONE', #14391, 1000.000000000000000 ) ;
#825 = CARTESIAN_POINT ( 'NONE',  ( 16.75000000000000000, -2.500000000000000000, -23.22168783648699986 ) ) ;
#826 = DIRECTION ( 'NONE',  ( 1.000000000000000000, 0.000000000000000000, 0.000000000000000000 ) ) ;
#827 = FACE_OUTER_BOUND ( 'NONE', #4879, .T. ) ;
#828 = DIRECTION ( 'NONE',  ( -0.000000000000000000, -0.000000000000000000, 1.000000000000000000 ) ) ;
#829 = DIRECTION ( 'NONE',  ( 0.08715574274766167695, 0.000000000000000000, -0.9961946980917453232 ) ) ;
#830 = CARTESIAN_POINT ( 'NONE',  ( 22.58164641901421632, 12.59999970914575940, -8.183940086454237317 ) ) ;
#831 = EDGE_LOOP ( 'NONE', ( #4724, #1877 ) ) ;
#832 = DIRECTION ( 'NONE',  ( 1.000000000000000000, 0.000000000000000000, 0.000000000000000000 ) ) ;
#833 = VECTOR ( 'NONE', #8086, 1000.000000000000000 ) ;
#834 = CIRCLE ( 'NONE', #7800, 10.49999999999999467 ) ;
#835 = ORIENTED_EDGE ( 'NONE', *, *, #11996, .T. ) ;
#836 = EDGE_LOOP ( 'NONE', ( #1705, #12143 ) ) ;
#837 = CARTESIAN_POINT ( 'NONE',  ( 0.9968050443165104024, -4.381875000000003517, 3.281628308787421844 ) ) ;
#838 = EDGE_LOOP ( 'NONE', ( #8455, #3676 ) ) ;
#839 = ORIENTED_EDGE ( 'NONE', *, *, #12386, .T. ) ;
#840 = VERTEX_POINT ( 'NONE', #10385 ) ;
#841 = CARTESIAN_POINT ( 'NONE',  ( 0.3497462729172694518, -6.233588562373080677, -3.541697392899130659 ) ) ;
#842 = CARTESIAN_POINT ( 'NONE',  ( 0.7624512442115692901, -0.8037500000000172840, -3.827857439461599398 ) ) ;
#843 = DIRECTION ( 'NONE',  ( -0.000000000000000000, 1.000000000000000000, -0.000000000000000000 ) ) ;
#844 = CARTESIAN_POINT ( 'NONE',  ( -0.001482159116125898214, -2.249999999999994227, -4.085353063378265759 ) ) ;
#845 = AXIS2_PLACEMENT_3D ( 'NONE', #10999, #1460, #3868 ) ;
#846 = VECTOR ( 'NONE', #239, 1000.000000000000000 ) ;
#847 = DIRECTION ( 'NONE',  ( 0.000000000000000000, 0.000000000000000000, -1.000000000000000000 ) ) ;
#848 = DIRECTION ( 'NONE',  ( -0.000000000000000000, 1.000000000000000000, -0.000000000000000000 ) ) ;
#849 = CARTESIAN_POINT ( 'NONE',  ( -4.296274425956841725, -0.5002988223950231017, 0.02453012155904704325 ) ) ;
#850 = CARTESIAN_POINT ( 'NONE',  ( -2.335396930795095471, -1.343749999999818368, -3.497180482087419051 ) ) ;
#851 = LINE ( 'NONE', #4429, #8047 ) ;
#852 = CARTESIAN_POINT ( 'NONE',  ( -76.26311196519618818, 67.29799558322736175, -81.84847958357697451 ) ) ;
#853 = CARTESIAN_POINT ( 'NONE',  ( -84.73238362643999722, 66.35306774555222376, -147.9984795835769944 ) ) ;
#854 = EDGE_LOOP ( 'NONE', ( #10172, #8366, #12990, #13556 ) ) ;
#855 = DIRECTION ( 'NONE',  ( 0.000000000000000000, 1.000000000000000000, 0.000000000000000000 ) ) ;
#856 = VERTEX_POINT ( 'NONE', #2014 ) ;
#857 = ORIENTED_EDGE ( 'NONE', *, *, #4793, .F. ) ;
#858 = VERTEX_POINT ( 'NONE', #852 ) ;
#859 = EDGE_CURVE ( 'NONE', #2988, #2847, #6988, .T. ) ;
#860 = DIRECTION ( 'NONE',  ( 0.000000000000000000, 0.000000000000000000, -1.000000000000000000 ) ) ;
#861 = AXIS2_PLACEMENT_3D ( 'NONE', #11815, #4836, #8324 ) ;
#862 = EDGE_CURVE ( 'NONE', #10484, #6682, #4430, .T. ) ;
#863 = LINE ( 'NONE', #638, #2101 ) ;
#864 = CARTESIAN_POINT ( 'NONE',  ( 33.35543536254877495, -3.618985300545106920, 6.000000000000001776 ) ) ;
#865 = CARTESIAN_POINT ( 'NONE',  ( -69.77438362644001302, 74.17411849586699191, -79.49847958357700861 ) ) ;
#866 = DIRECTION ( 'NONE',  ( -0.000000000000000000, 0.000000000000000000, 1.000000000000000000 ) ) ;
#867 = CARTESIAN_POINT ( 'NONE',  ( -3.252405029756590515, -0.4995676945082676568, 2.664931962243846097 ) ) ;
#868 = DIRECTION ( 'NONE',  ( 0.000000000000000000, 0.000000000000000000, -1.000000000000000000 ) ) ;
#869 = AXIS2_PLACEMENT_3D ( 'NONE', #14614, #1744, #12312 ) ;
#870 = EDGE_LOOP ( 'NONE', ( #7613, #12898, #857 ) ) ;
#871 = AXIS2_PLACEMENT_3D ( 'NONE', #13865, #1924, #4183 ) ;
#872 = CYLINDRICAL_SURFACE ( 'NONE', #9576, 1.999999999999986233 ) ;
#873 = EDGE_LOOP ( 'NONE', ( #4886, #278 ) ) ;
#874 = ORIENTED_EDGE ( 'NONE', *, *, #9028, .F. ) ;
#875 = CARTESIAN_POINT ( 'NONE',  ( -80.52077156573417938, 103.6741184958669777, -79.59847958357700293 ) ) ;
#876 = EDGE_CURVE ( 'NONE', #411, #12032, #15182, .T. ) ;
#877 = VERTEX_POINT ( 'NONE', #9379 ) ;
#878 = CARTESIAN_POINT ( 'NONE',  ( 0.001121683909886545937, -1.249999999999918066, -4.217678074926116238 ) ) ;
#879 = ORIENTED_EDGE ( 'NONE', *, *, #5951, .F. ) ;
#880 = CARTESIAN_POINT ( 'NONE',  ( 0.001080389160871208457, -2.249213562373011843, -4.085999009053598918 ) ) ;
#881 = AXIS2_PLACEMENT_3D ( 'NONE', #3446, #7110, #2276 ) ;
#882 = FACE_OUTER_BOUND ( 'NONE', #4907, .T. ) ;
#883 = CARTESIAN_POINT ( 'NONE',  ( -73.64736697264537213, 89.17411849586700612, -57.99847958357699440 ) ) ;
#884 = APPLICATION_CONTEXT ( 'automotive_design' ) ;
#885 = DIRECTION ( 'NONE',  ( 0.8660254037844387076, 0.4999999999999998890, 0.000000000000000000 ) ) ;
#886 = EDGE_CURVE ( 'NONE', #2365, #2303, #929, .T. ) ;
#887 = DIRECTION ( 'NONE',  ( 1.000000000000000000, 0.000000000000000000, 0.000000000000000000 ) ) ;
#888 = EDGE_CURVE ( 'NONE', #1688, #9382, #4871, .T. ) ;
#889 = VECTOR ( 'NONE', #2242, 1000.000000000000000 ) ;
#890 = DIRECTION ( 'NONE',  ( -0.000000000000000000, -0.000000000000000000, 1.000000000000000000 ) ) ;
#891 = FACE_OUTER_BOUND ( 'NONE', #14981, .T. ) ;
#892 = AXIS2_PLACEMENT_3D ( 'NONE', #9092, #5399, #943 ) ;
#893 = AXIS2_PLACEMENT_3D ( 'NONE', #10244, #13754, #3201 ) ;
#894 = EDGE_CURVE ( 'NONE', #9154, #8986, #5120, .T. ) ;
#895 = ORIENTED_EDGE ( 'NONE', *, *, #1284, .T. ) ;
#896 = CARTESIAN_POINT ( 'NONE',  ( 2.372013019084901586, -4.859374999999952927, 2.891838320553053343 ) ) ;
#897 = VERTEX_POINT ( 'NONE', #15111 ) ;
#898 = ADVANCED_FACE ( 'NONE', ( #3412 ), #4578, .F. ) ;
#899 = ADVANCED_FACE ( 'NONE', ( #13961 ), #12648, .F. ) ;
#900 = CARTESIAN_POINT ( 'NONE',  ( 2.822884439542639790, -2.694375000000075460, -2.318423337397389261 ) ) ;
#901 = AXIS2_PLACEMENT_3D ( 'NONE', #8143, #62, #9295 ) ;
#902 = CARTESIAN_POINT ( 'NONE',  ( -69.77438362644001302, 82.17411849586700612, -80.44847958357698303 ) ) ;
#903 = CARTESIAN_POINT ( 'NONE',  ( -69.77438362644001302, 82.17411849586700612, -81.84847958357697451 ) ) ;
#904 = ADVANCED_FACE ( 'NONE', ( #10542 ), #4128, .F. ) ;
#905 = DIRECTION ( 'NONE',  ( 0.000000000000000000, 0.000000000000000000, -1.000000000000000000 ) ) ;
#906 = PLANE ( 'NONE',  #4282 ) ;
#907 = FACE_OUTER_BOUND ( 'NONE', #7178, .T. ) ;
#908 = DIRECTION ( 'NONE',  ( 0.000000000000000000, 1.000000000000000000, 0.000000000000000000 ) ) ;
#909 = ORIENTED_EDGE ( 'NONE', *, *, #15198, .F. ) ;
#910 = CARTESIAN_POINT ( 'NONE',  ( -57.02438362643999170, 65.17411849586700612, -149.9984795835770228 ) ) ;
#911 = CONICAL_SURFACE ( 'NONE', #5404, 2.500000000000002220, 1.029744258676651425 ) ;
#912 = EDGE_CURVE ( 'NONE', #3825, #2695, #14769, .T. ) ;
#913 = VERTEX_POINT ( 'NONE', #14963 ) ;
#914 = TOROIDAL_SURFACE ( 'NONE', #14545, 2.931404194366992400, 0.5000000000000000000 ) ;
#915 = ORIENTED_EDGE ( 'NONE', *, *, #5346, .F. ) ;
#916 = CARTESIAN_POINT ( 'NONE',  ( -0.6836773592642515496, -3.866249999999994635, -3.430425219284938265 ) ) ;
#917 = ORIENTED_EDGE ( 'NONE', *, *, #10777, .F. ) ;
#918 = ORIENTED_EDGE ( 'NONE', *, *, #3458, .F. ) ;
#919 = EDGE_LOOP ( 'NONE', ( #10109, #1775, #5406, #6735 ) ) ;
#920 = CARTESIAN_POINT ( 'NONE',  ( -2.836763133589473629, -5.389838562373330255, -2.329300430828157076 ) ) ;
#921 = CARTESIAN_POINT ( 'NONE',  ( -3.916933349122106112, -0.1162499999999876271, 0.7806084585172713419 ) ) ;
#922 = CARTESIAN_POINT ( 'NONE',  ( -3.119281932368198618, -5.304704016482149953, 1.429041148738060985 ) ) ;
#923 = CARTESIAN_POINT ( 'NONE',  ( 0.4017167453136591404, -2.234374999999921396, -4.067671435978028605 ) ) ;
#924 = CARTESIAN_POINT ( 'NONE',  ( -59.27438362644000591, 82.17411849586700612, -82.44847958357698303 ) ) ;
#925 = DIRECTION ( 'NONE',  ( -1.000000000000000000, 1.734723475976808672E-15, 0.000000000000000000 ) ) ;
#926 = VECTOR ( 'NONE', #11580, 1000.000000000000000 ) ;
#927 = LINE ( 'NONE', #10383, #12346 ) ;
#928 = DIRECTION ( 'NONE',  ( -0.000000000000000000, -0.000000000000000000, 1.000000000000000000 ) ) ;
#929 = LINE ( 'NONE', #10314, #7602 ) ;
#930 = FACE_OUTER_BOUND ( 'NONE', #9434, .T. ) ;
#931 = ORIENTED_EDGE ( 'NONE', *, *, #748, .T. ) ;
#932 = CARTESIAN_POINT ( 'NONE',  ( -14.25000000000000000, -0.2038245569916330158, -23.22168783648699986 ) ) ;
#933 = ORIENTED_EDGE ( 'NONE', *, *, #4607, .F. ) ;
#934 = ORIENTED_EDGE ( 'NONE', *, *, #1194, .T. ) ;
#935 = ORIENTED_EDGE ( 'NONE', *, *, #8658, .T. ) ;
#936 = UNCERTAINTY_MEASURE_WITH_UNIT (LENGTH_MEASURE( 1.000000000000000082E-05 ), #9896, 'distance_accuracy_value', 'NONE');
#937 = AXIS2_PLACEMENT_3D ( 'NONE', #2010, #6986, #10226 ) ;
#938 = LINE ( 'NONE', #14971, #4017 ) ;
#939 = CARTESIAN_POINT ( 'NONE',  ( 0.0008557816480155369665, -4.835000000000089670, -3.369777484087370212 ) ) ;
#940 = CARTESIAN_POINT ( 'NONE',  ( -35.27438362644000591, 111.1741184958670061, -79.49847958357700861 ) ) ;
#941 = DIRECTION ( 'NONE',  ( 0.000000000000000000, 0.000000000000000000, 1.000000000000000000 ) ) ;
#942 = CARTESIAN_POINT ( 'NONE',  ( -88.81638362644100937, 97.99516924618178848, -147.9984795835769944 ) ) ;
#943 = DIRECTION ( 'NONE',  ( 1.000000000000000000, 0.000000000000000000, 0.000000000000000000 ) ) ;
#944 = B_SPLINE_CURVE_WITH_KNOTS ( 'NONE', 3,
 ( #11651, #15208, #10718, #83 ),
 .UNSPECIFIED., .F., .F.,
 ( 4, 4 ),
 ( 0.002598307151460989371, 0.005196383362814305240 ),
 .UNSPECIFIED. ) ;
#945 = CARTESIAN_POINT ( 'NONE',  ( -35.27438362644000591, 111.1741184958670061, -67.49847958357700861 ) ) ;
#946 = DIRECTION ( 'NONE',  ( -0.000000000000000000, 0.7071067811865441310, 0.7071067811865510144 ) ) ;
#947 = PLANE ( 'NONE',  #13258 ) ;
#948 = AXIS2_PLACEMENT_3D ( 'NONE', #13719, #7962, #10362 ) ;
#949 = ORIENTED_EDGE ( 'NONE', *, *, #6427, .T. ) ;
#950 = DIRECTION ( 'NONE',  ( 0.000000000000000000, 0.000000000000000000, 1.000000000000000000 ) ) ;
#951 = ADVANCED_FACE ( 'NONE', ( #9079 ), #3778, .F. ) ;
#952 = ORIENTED_EDGE ( 'NONE', *, *, #14604, .F. ) ;
#953 = VERTEX_POINT ( 'NONE', #6361 ) ;
#954 = CARTESIAN_POINT ( 'NONE',  ( -52.77438362644100067, 99.17411849586700612, -145.4984795835769944 ) ) ;
#955 = ORIENTED_EDGE ( 'NONE', *, *, #243, .F. ) ;
#956 = CARTESIAN_POINT ( 'NONE',  ( 0.4056240317150583419, -1.765625000000045741, 4.129595427369183724 ) ) ;
#957 = VERTEX_POINT ( 'NONE', #9741 ) ;
#958 = CARTESIAN_POINT ( 'NONE',  ( -0.3927583221446535044, -2.733588562373027830, 4.002660525033727268 ) ) ;
#959 = VECTOR ( 'NONE', #10043, 1000.000000000000000 ) ;
#960 = CARTESIAN_POINT ( 'NONE',  ( 15.50000000000000000, -0.4000000000005274892, -25.79999999999946780 ) ) ;
#961 = CARTESIAN_POINT ( 'NONE',  ( -15.50000000000000000, -5.000000000000000000, -26.00000000000000000 ) ) ;
#962 = CARTESIAN_POINT ( 'NONE',  ( -86.77438362643999881, 62.81621999649657084, -147.9984795835769944 ) ) ;
#963 = ADVANCED_FACE ( 'NONE', ( #4948 ), #6368, .T. ) ;
#964 = CARTESIAN_POINT ( 'NONE',  ( -86.77438362644001302, 65.17411849586700612, -145.4984795835769660 ) ) ;
#965 = ORIENTED_EDGE ( 'NONE', *, *, #6895, .T. ) ;
#966 = DIRECTION ( 'NONE',  ( 0.000000000000000000, -1.000000000000000000, -0.000000000000000000 ) ) ;
#967 = EDGE_CURVE ( 'NONE', #10723, #12753, #13779, .T. ) ;
#968 = DIRECTION ( 'NONE',  ( 0.003614861529253208996, 0.000000000000000000, -0.9999934663667179313 ) ) ;
#969 =( NAMED_UNIT ( * ) SI_UNIT ( $, .STERADIAN. ) SOLID_ANGLE_UNIT ( ) );
#970 = ORIENTED_EDGE ( 'NONE', *, *, #13625, .T. ) ;
#971 = DIRECTION ( 'NONE',  ( 0.000000000000000000, 1.000000000000000000, 0.000000000000000000 ) ) ;
#972 = CARTESIAN_POINT ( 'NONE',  ( 3.852585042300790796, -0.6162500000000914469, -0.7652758215885019366 ) ) ;
#973 = ORIENTED_EDGE ( 'NONE', *, *, #13857, .F. ) ;
#974 = CARTESIAN_POINT ( 'NONE',  ( 3.244093391032126572, -2.506875000000020837, 1.732468392772068544 ) ) ;
#975 = EDGE_CURVE ( 'NONE', #6718, #10037, #7105, .T. ) ;
#976 = CARTESIAN_POINT ( 'NONE',  ( -69.77438362644001302, 82.17411849586700612, -80.44847958357698303 ) ) ;
#977 = CARTESIAN_POINT ( 'NONE',  ( 3.676486008612421585, -0.4995676945082496712, 1.453030271339659008 ) ) ;
#978 = SURFACE_SIDE_STYLE ('',( #15322 ) ) ;
#979 = CARTESIAN_POINT ( 'NONE',  ( -80.52077156573417938, 59.67411849586701322, -15.85886927678779834 ) ) ;
#980 = EDGE_CURVE ( 'NONE', #2847, #1167, #402, .T. ) ;
#981 = LINE ( 'NONE', #3393, #10692 ) ;
#982 = EDGE_CURVE ( 'NONE', #7121, #1333, #12154, .T. ) ;
#983 = EDGE_LOOP ( 'NONE', ( #1998, #985 ) ) ;
#984 = PLANE ( 'NONE',  #7031 ) ;
#985 = ORIENTED_EDGE ( 'NONE', *, *, #10099, .T. ) ;
#986 = ORIENTED_EDGE ( 'NONE', *, *, #6710, .F. ) ;
#987 = CARTESIAN_POINT ( 'NONE',  ( 1.592243150387700146, -4.756875000000070131, -2.981552405995577804 ) ) ;
#988 = ORIENTED_EDGE ( 'NONE', *, *, #10578, .F. ) ;
#989 = B_SPLINE_CURVE_WITH_KNOTS ( 'NONE', 3,
 ( #4367, #11577, #2032, #4517, #9091, #5770, #6928, #11351 ),
 .UNSPECIFIED., .F., .F.,
 ( 4, 2, 2, 4 ),
 ( 0.04315383327197147567, 0.04413750674005950669, 0.04512118020814753772, 0.04708852714432359976 ),
 .UNSPECIFIED. ) ;
#990 = ORIENTED_EDGE ( 'NONE', *, *, #10629, .F. ) ;
#991 = ORIENTED_EDGE ( 'NONE', *, *, #11903, .T. ) ;
#992 = CARTESIAN_POINT ( 'NONE',  ( 3.431607731776029180, -5.061713562373087782, -1.420375347272441857 ) ) ;
#993 = EDGE_CURVE ( 'NONE', #8371, #10438, #9314, .T. ) ;
#994 = CARTESIAN_POINT ( 'NONE',  ( 3.049996619588533520, -0.4756250000000030176, 2.504408566260877489 ) ) ;
#995 = CARTESIAN_POINT ( 'NONE',  ( -3.582436959730881831, -2.421875000000131450, -1.916069189016956331 ) ) ;
#996 = FACE_OUTER_BOUND ( 'NONE', #7197, .T. ) ;
#997 = EDGE_CURVE ( 'NONE', #8110, #14910, #1607, .T. ) ;
#998 = FACE_OUTER_BOUND ( 'NONE', #11079, .T. ) ;
#999 = DIRECTION ( 'NONE',  ( -0.000000000000000000, -1.000000000000000000, -0.000000000000000000 ) ) ;
#1000 = CARTESIAN_POINT ( 'NONE',  ( 68.41329019055577021, 5.000000000000000000, 91.50956111919110469 ) ) ;
#1001 = DIRECTION ( 'NONE',  ( -1.669238443041288662E-16, -4.259781144855898747E-31, -1.000000000000000000 ) ) ;
#1002 = CARTESIAN_POINT ( 'NONE',  ( 3.388605160257775140, -4.569374999999831211, 0.3324735777646720680 ) ) ;
#1003 = FACE_OUTER_BOUND ( 'NONE', #12432, .T. ) ;
#1004 = ADVANCED_FACE ( 'NONE', ( #8590 ), #11077, .T. ) ;
#1005 = ORIENTED_EDGE ( 'NONE', *, *, #9618, .T. ) ;
#1006 = CYLINDRICAL_SURFACE ( 'NONE', #12711, 4.709525205202999665 ) ;
#1007 = ORIENTED_EDGE ( 'NONE', *, *, #11900, .T. ) ;
#1008 = ORIENTED_EDGE ( 'NONE', *, *, #6965, .F. ) ;
#1009 = EDGE_LOOP ( 'NONE', ( #14869, #9513, #7261, #3118 ) ) ;
#1010 = VECTOR ( 'NONE', #6669, 1000.000000000000000 ) ;
#1011 = DIRECTION ( 'NONE',  ( 0.000000000000000000, 0.000000000000000000, 1.000000000000000000 ) ) ;
#1012 = CARTESIAN_POINT ( 'NONE',  ( 3.136514378097080780, -4.647499999999995524, -1.298252083346796759 ) ) ;
#1013 = DIRECTION ( 'NONE',  ( -0.08715574274766167695, 0.000000000000000000, 0.9961946980917453232 ) ) ;
#1014 = DIRECTION ( 'NONE',  ( 0.000000000000000000, 0.000000000000000000, -1.000000000000000000 ) ) ;
#1015 = DIRECTION ( 'NONE',  ( 0.000000000000000000, 0.000000000000000000, 1.000000000000000000 ) ) ;
#1016 = DIRECTION ( 'NONE',  ( -1.000000000000000000, -0.000000000000000000, -0.000000000000000000 ) ) ;
#1017 = CIRCLE ( 'NONE', #525, 4.250000000000003553 ) ;
#1018 = CARTESIAN_POINT ( 'NONE',  ( -84.27438362644100778, 99.17411849586700612, -79.59847958357700293 ) ) ;
#1019 = DIRECTION ( 'NONE',  ( 1.000000000000000000, 0.000000000000000000, 0.000000000000000000 ) ) ;
#1020 = CARTESIAN_POINT ( 'NONE',  ( -48.52438362643999881, 65.17411849586700612, -182.2484795835770228 ) ) ;
#1021 = DIRECTION ( 'NONE',  ( 0.000000000000000000, 0.000000000000000000, -1.000000000000000000 ) ) ;
#1022 = VECTOR ( 'NONE', #491, 1000.000000000000000 ) ;
#1023 = ORIENTED_EDGE ( 'NONE', *, *, #811, .T. ) ;
#1024 = DIRECTION ( 'NONE',  ( -1.287488025362404182E-15, -1.000000000000000000, 0.000000000000000000 ) ) ;
#1025 = EDGE_LOOP ( 'NONE', ( #12553, #9996 ) ) ;
#1026 = ORIENTED_EDGE ( 'NONE', *, *, #3001, .F. ) ;
#1027 = CARTESIAN_POINT ( 'NONE',  ( -77.52077156573416516, 103.6741184958669777, -152.4984795835769944 ) ) ;
#1028 = ORIENTED_EDGE ( 'NONE', *, *, #1342, .F. ) ;
#1029 = AXIS2_PLACEMENT_3D ( 'NONE', #10896, #5000, #9714 ) ;
#1030 = CARTESIAN_POINT ( 'NONE',  ( -3.998008487304611336, -1.546875000000091038, 1.214361949261595131 ) ) ;
#1031 = ORIENTED_EDGE ( 'NONE', *, *, #11429, .F. ) ;
#1032 = CARTESIAN_POINT ( 'NONE',  ( 3.914479021157896810, -2.967963562373050923, 0.7771573004458622869 ) ) ;
#1033 =( GEOMETRIC_REPRESENTATION_CONTEXT ( 3 ) GLOBAL_UNCERTAINTY_ASSIGNED_CONTEXT ( ( #9938 ) ) GLOBAL_UNIT_ASSIGNED_CONTEXT ( ( #4952, #11854, #14327 ) ) REPRESENTATION_CONTEXT ( 'NONE', 'WORKASPACE' ) );
#1034 = FACE_BOUND ( 'NONE', #15170, .T. ) ;
#1035 = CIRCLE ( 'NONE', #5506, 10.50000000000000178 ) ;
#1036 = CARTESIAN_POINT ( 'NONE',  ( -80.52077156573417938, 110.1741184958670061, -15.85886927678779834 ) ) ;
#1037 = DIRECTION ( 'NONE',  ( -1.000000000000000000, 0.000000000000000000, 0.000000000000000000 ) ) ;
#1038 = CIRCLE ( 'NONE', #9708, 4.000000000000000000 ) ;
#1039 = CARTESIAN_POINT ( 'NONE',  ( -90.85838362644000199, 65.17411849586700612, -147.9984795835769944 ) ) ;
#1040 = ORIENTED_EDGE ( 'NONE', *, *, #12700, .T. ) ;
#1041 = CARTESIAN_POINT ( 'NONE',  ( 3.530157234965975555, -5.226201182446649440, -2.246195850846843811E-13 ) ) ;
#1042 = CARTESIAN_POINT ( 'NONE',  ( 17.14647606710965988, -3.654413409933304102, 0.2671853888517377595 ) ) ;
#1043 = AXIS2_PLACEMENT_3D ( 'NONE', #2565, #10946, #14427 ) ;
#1044 = ORIENTED_EDGE ( 'NONE', *, *, #3572, .F. ) ;
#1045 = CARTESIAN_POINT ( 'NONE',  ( -3.637955631634660403, -5.500000000000000000, 0.000000000000000000 ) ) ;
#1046 = ORIENTED_EDGE ( 'NONE', *, *, #8355, .T. ) ;
#1047 = EDGE_CURVE ( 'NONE', #14750, #8289, #1453, .T. ) ;
#1048 = AXIS2_PLACEMENT_3D ( 'NONE', #7609, #8905, #462 ) ;
#1049 = CARTESIAN_POINT ( 'NONE',  ( 1.394838545734166990, -2.772499999999996856, -3.364978284447634582 ) ) ;
#1050 = DIRECTION ( 'NONE',  ( 1.000000000000000000, 0.000000000000000000, 0.000000000000000000 ) ) ;
#1051 = DIRECTION ( 'NONE',  ( -1.747085166004344019E-15, 1.000000000000000000, -0.000000000000000000 ) ) ;
#1052 = DIRECTION ( 'NONE',  ( -0.9961946980917453232, 7.200509705930739692E-17, -0.08715574274766156593 ) ) ;
#1053 = CARTESIAN_POINT ( 'NONE',  ( -59.02799568714584666, 59.67411849586701322, -152.4984795835769944 ) ) ;
#1054 = LINE ( 'NONE', #1990, #7758 ) ;
#1055 = CARTESIAN_POINT ( 'NONE',  ( -52.77438362644000591, 99.17411849586700612, -145.4984795835769660 ) ) ;
#1056 = LINE ( 'NONE', #11850, #4509 ) ;
#1057 = AXIS2_PLACEMENT_3D ( 'NONE', #12391, #5489, #1683 ) ;
#1058 = VERTEX_POINT ( 'NONE', #10992 ) ;
#1059 = DIRECTION ( 'NONE',  ( 0.000000000000000000, 0.000000000000000000, 1.000000000000000000 ) ) ;
#1060 = ORIENTED_EDGE ( 'NONE', *, *, #10858, .T. ) ;
#1061 = ORIENTED_EDGE ( 'NONE', *, *, #4996, .F. ) ;
#1062 = CARTESIAN_POINT ( 'NONE',  ( -3.196762997434542175, -4.147500000000007958, 1.325534829466322062 ) ) ;
#1063 = ORIENTED_EDGE ( 'NONE', *, *, #10334, .F. ) ;
#1064 = EDGE_LOOP ( 'NONE', ( #13321, #2642, #1345, #3553 ) ) ;
#1065 = CIRCLE ( 'NONE', #9480, 1.199999999999999734 ) ;
#1066 = ADVANCED_FACE ( 'NONE', ( #2532, #8734 ), #13253, .T. ) ;
#1067 = VERTEX_POINT ( 'NONE', #2845 ) ;
#1068 = CARTESIAN_POINT ( 'NONE',  ( -0.3692575584143804046, -4.733588562373068243, 3.739163940647424855 ) ) ;
#1069 = DIRECTION ( 'NONE',  ( -0.7071067811865500152, -0.000000000000000000, -0.7071067811865451302 ) ) ;
#1070 = EDGE_CURVE ( 'NONE', #4318, #8552, #8080, .T. ) ;
#1071 = AXIS2_PLACEMENT_3D ( 'NONE', #14411, #9758, #14493 ) ;
#1072 = DIRECTION ( 'NONE',  ( 0.000000000000000000, -0.000000000000000000, 1.000000000000000000 ) ) ;
#1073 = DIRECTION ( 'NONE',  ( -0.4999999999999832356, 0.000000000000000000, -0.8660254037844483666 ) ) ;
#1074 = DIRECTION ( 'NONE',  ( -1.000000000000000000, 0.000000000000000000, 0.000000000000000000 ) ) ;
#1075 = B_SPLINE_CURVE_WITH_KNOTS ( 'NONE', 3,
 ( #9010, #12658, #3045, #2027, #15050, #12813 ),
 .UNSPECIFIED., .F., .F.,
 ( 4, 2, 4 ),
 ( 0.0002380763768129734448, 0.7291065797294589146, 1.457975083082104995 ),
 .UNSPECIFIED. ) ;
#1076 = LINE ( 'NONE', #9376, #15049 ) ;
#1077 = DIRECTION ( 'NONE',  ( -9.422394424380278809E-16, 1.000000000000000000, -0.000000000000000000 ) ) ;
#1078 = DIRECTION ( 'NONE',  ( 0.000000000000000000, 0.000000000000000000, 1.000000000000000000 ) ) ;
#1079 = CIRCLE ( 'NONE', #3812, 1.250000000000001110 ) ;
#1080 = CARTESIAN_POINT ( 'NONE',  ( 17.16405274069114739, 3.654316742536410256, 0.2664120436859874763 ) ) ;
#1081 = AXIS2_PLACEMENT_3D ( 'NONE', #13581, #5203, #2785 ) ;
#1082 = CARTESIAN_POINT ( 'NONE',  ( 1.682902201845278611, -5.420849775684215999, 2.811263474311217259 ) ) ;
#1083 = LINE ( 'NONE', #4580, #13952 ) ;
#1084 = ADVANCED_FACE ( 'NONE', ( #12232 ), #7593, .F. ) ;
#1085 = ORIENTED_EDGE ( 'NONE', *, *, #2902, .T. ) ;
#1086 = EDGE_CURVE ( 'NONE', #8835, #6563, #8583, .T. ) ;
#1087 = CARTESIAN_POINT ( 'NONE',  ( -79.02077156573416516, 60.67411849586702743, -79.59847958357700293 ) ) ;
#1088 = ORIENTED_EDGE ( 'NONE', *, *, #8768, .F. ) ;
#1089 = ORIENTED_EDGE ( 'NONE', *, *, #7043, .T. ) ;
#1090 = ORIENTED_EDGE ( 'NONE', *, *, #6419, .T. ) ;
#1091 = EDGE_CURVE ( 'NONE', #2409, #160, #8338, .T. ) ;
#1092 = DIRECTION ( 'NONE',  ( -0.8660254037844387076, -0.4999999999999998890, 0.000000000000000000 ) ) ;
#1093 = CARTESIAN_POINT ( 'NONE',  ( -1.685726645313963434, -3.256874999999974651, 3.156579729352138486 ) ) ;
#1094 = AXIS2_PLACEMENT_3D ( 'NONE', #12697, #4639, #6961 ) ;
#1095 = EDGE_CURVE ( 'NONE', #11388, #11166, #13173, .T. ) ;
#1096 = EDGE_CURVE ( 'NONE', #1293, #13867, #5378, .T. ) ;
#1097 = CARTESIAN_POINT ( 'NONE',  ( 35.35543536254876074, -3.618985300545107364, 6.000000000000001776 ) ) ;
#1098 = CARTESIAN_POINT ( 'NONE',  ( 3.291891004236185747, -4.921874999999971578, 1.757997479805845975 ) ) ;
#1099 = CARTESIAN_POINT ( 'NONE',  ( -14.25000000000000000, -0.2038245569916330158, 23.22168783648699986 ) ) ;
#1100 = DIRECTION ( 'NONE',  ( 1.000000000000000000, 0.000000000000000000, 0.000000000000000000 ) ) ;
#1101 = FACE_OUTER_BOUND ( 'NONE', #6719, .T. ) ;
#1102 = CARTESIAN_POINT ( 'NONE',  ( 16.75000000000000000, -2.500000000000000000, 21.77831216351300014 ) ) ;
#1103 = CARTESIAN_POINT ( 'NONE',  ( 57.41329019055577021, 0.000000000000000000, 129.5095611191910621 ) ) ;
#1104 = CARTESIAN_POINT ( 'NONE',  ( 21.98164641901421135, 11.99999970914576330, -8.733587956314005751 ) ) ;
#1105 = ORIENTED_EDGE ( 'NONE', *, *, #13994, .F. ) ;
#1106 = CARTESIAN_POINT ( 'NONE',  ( -84.73238362643999722, 66.35306774555222376, -150.4984795835770228 ) ) ;
#1107 = VECTOR ( 'NONE', #14384, 1000.000000000000114 ) ;
#1108 = ORIENTED_EDGE ( 'NONE', *, *, #8495, .F. ) ;
#1109 = ORIENTED_EDGE ( 'NONE', *, *, #4097, .F. ) ;
#1110 = CARTESIAN_POINT ( 'NONE',  ( -1.629699455448989389E-14, 8.699999999999999289, 5.655858585055787181E-29 ) ) ;
#1111 = VERTEX_POINT ( 'NONE', #4315 ) ;
#1112 = EDGE_CURVE ( 'NONE', #4275, #181, #10269, .T. ) ;
#1113 = DIRECTION ( 'NONE',  ( -1.000000000000000000, 0.000000000000000000, 0.000000000000000000 ) ) ;
#1114 = VERTEX_POINT ( 'NONE', #12546 ) ;
#1115 = CARTESIAN_POINT ( 'NONE',  ( -3.565751477134541769, -2.577338562373002961, 1.904724266850964520 ) ) ;
#1116 = CARTESIAN_POINT ( 'NONE',  ( 15.50000000000000000, 0.000000000000000000, -22.50000000000000000 ) ) ;
#1117 = LINE ( 'NONE', #1036, #6362 ) ;
#1118 = AXIS2_PLACEMENT_3D ( 'NONE', #3027, #10142, #13735 ) ;
#1119 = FACE_OUTER_BOUND ( 'NONE', #655, .T. ) ;
#1120 = VECTOR ( 'NONE', #11401, 1000.000000000000000 ) ;
#1121 = DIRECTION ( 'NONE',  ( -7.395386697914957063E-16, -1.000000000000000000, 0.000000000000000000 ) ) ;
#1122 = ORIENTED_EDGE ( 'NONE', *, *, #14847, .T. ) ;
#1123 = DIRECTION ( 'NONE',  ( 0.000000000000000000, 0.000000000000000000, 1.000000000000000000 ) ) ;
#1124 = PLANE ( 'NONE',  #4523 ) ;
#1125 = VECTOR ( 'NONE', #12355, 1000.000000000000000 ) ;
#1126 = ORIENTED_EDGE ( 'NONE', *, *, #331, .T. ) ;
#1127 = B_SPLINE_CURVE_WITH_KNOTS ( 'NONE', 3,
 ( #8403, #10724, #13144, #12054, #4922, #3901, #1422, #1569, #2574, #2494 ),
 .UNSPECIFIED., .F., .F.,
 ( 4, 2, 2, 2, 4 ),
 ( 0.000000000000000000, 0.0002904196669106299503, 0.0005808393338212599006, 0.0008712590007318899051, 0.001161678667642519801 ),
 .UNSPECIFIED. ) ;
#1128 = CIRCLE ( 'NONE', #11785, 3.968749999999992895 ) ;
#1129 = CARTESIAN_POINT ( 'NONE',  ( 2.507317702870420106, -0.4443749999999629940, 3.052905756198935894 ) ) ;
#1130 = EDGE_LOOP ( 'NONE', ( #13827, #11841, #4280 ) ) ;
#1131 = CONICAL_SURFACE ( 'NONE', #11533, 3.637955631634646192, 0.1308996938995775905 ) ;
#1132 = CARTESIAN_POINT ( 'NONE',  ( -2.557519727433407386, -2.960000000000007958, -2.558839988362045403 ) ) ;
#1133 = CARTESIAN_POINT ( 'NONE',  ( -48.27438362644000591, 99.17411849586700612, -86.49847958357699440 ) ) ;
#1134 = VECTOR ( 'NONE', #11888, 1000.000000000000000 ) ;
#1135 = LINE ( 'NONE', #8276, #3090 ) ;
#1136 = AXIS2_PLACEMENT_3D ( 'NONE', #1177, #11811, #1248 ) ;
#1137 = CARTESIAN_POINT ( 'NONE',  ( 37.35543536254874653, -3.618985300545107364, 0.000000000000000000 ) ) ;
#1138 = DIRECTION ( 'NONE',  ( 0.000000000000000000, 1.000000000000000000, 0.000000000000000000 ) ) ;
#1139 = CIRCLE ( 'NONE', #5618, 5.499999999999998224 ) ;
#1140 = DIRECTION ( 'NONE',  ( 0.000000000000000000, 1.000000000000000000, 0.000000000000000000 ) ) ;
#1141 = DIRECTION ( 'NONE',  ( 0.000000000000000000, 1.000000000000000000, 0.000000000000000000 ) ) ;
#1142 = ORIENTED_EDGE ( 'NONE', *, *, #4184, .T. ) ;
#1143 = DIRECTION ( 'NONE',  ( 0.000000000000000000, -4.130293990420970006E-17, 1.000000000000000000 ) ) ;
#1144 = EDGE_CURVE ( 'NONE', #12791, #11036, #7466, .T. ) ;
#1145 = ORIENTED_EDGE ( 'NONE', *, *, #13426, .T. ) ;
#1146 = ORIENTED_EDGE ( 'NONE', *, *, #9815, .F. ) ;
#1147 = CARTESIAN_POINT ( 'NONE',  ( 3.136514378097081224, -4.647499999999995524, -1.298252083346754793 ) ) ;
#1148 = EDGE_LOOP ( 'NONE', ( #12567, #12427, #8900, #13200 ) ) ;
#1149 = AXIS2_PLACEMENT_3D ( 'NONE', #2170, #13884, #3253 ) ;
#1150 = EDGE_LOOP ( 'NONE', ( #965, #3065, #8473, #1387, #1741, #5883 ) ) ;
#1151 = ORIENTED_EDGE ( 'NONE', *, *, #12378, .T. ) ;
#1152 = VECTOR ( 'NONE', #13066, 1000.000000000000000 ) ;
#1153 = CARTESIAN_POINT ( 'NONE',  ( -1.797749598780369329, -4.327338562373237885, -3.360391230360182835 ) ) ;
#1154 = DIRECTION ( 'NONE',  ( 0.000000000000000000, 0.000000000000000000, -1.000000000000000000 ) ) ;
#1155 = CARTESIAN_POINT ( 'NONE',  ( -13.41835358098578723, 11.99999970914575975, 0.2664120436859911956 ) ) ;
#1156 = DIRECTION ( 'NONE',  ( 9.422394424380274864E-16, -1.000000000000000000, 0.000000000000000000 ) ) ;
#1157 = CARTESIAN_POINT ( 'NONE',  ( -4.522482571421199360, 11.99999970914574021, 70.03692566716181034 ) ) ;
#1158 = DIRECTION ( 'NONE',  ( 1.000000000000000000, 0.000000000000000000, 0.000000000000000000 ) ) ;
#1159 = AXIS2_PLACEMENT_3D ( 'NONE', #3987, #8718, #6116 ) ;
#1160 = DIRECTION ( 'NONE',  ( 0.000000000000000000, 0.000000000000000000, -1.000000000000000000 ) ) ;
#1161 = EDGE_CURVE ( 'NONE', #6610, #6972, #7948, .T. ) ;
#1162 = CARTESIAN_POINT ( 'NONE',  ( -2.669536895096369378, -4.194375000000057696, 2.192493760422927984 ) ) ;
#1163 = CARTESIAN_POINT ( 'NONE',  ( -4.522482571421199360, -11.58578672848118352, 70.03692566716176771 ) ) ;
#1164 = AXIS2_PLACEMENT_3D ( 'NONE', #3408, #11789, #1074 ) ;
#1165 = EDGE_LOOP ( 'NONE', ( #2623, #10956, #13964, #3494 ) ) ;
#1166 = CARTESIAN_POINT ( 'NONE',  ( -14.45313394609757118, -0.2715358723599894386, -23.33896727494798284 ) ) ;
#1167 = VERTEX_POINT ( 'NONE', #7885 ) ;
#1168 = ORIENTED_EDGE ( 'NONE', *, *, #4774, .F. ) ;
#1169 = ORIENTED_EDGE ( 'NONE', *, *, #7747, .F. ) ;
#1170 = B_SPLINE_CURVE_WITH_KNOTS ( 'NONE', 3,
 ( #4775, #10827, #9570, #7117, #1203, #3612, #8349, #6037, #14311, #8418 ),
 .UNSPECIFIED., .F., .F.,
 ( 4, 2, 2, 2, 4 ),
 ( -1.214224233790302196E-05, 0.0002824113887451626783, 0.0005769650198282283904, 0.0008715186509112941024, 0.001166072281994359923 ),
 .UNSPECIFIED. ) ;
#1171 = CARTESIAN_POINT ( 'NONE',  ( 3.389189273868536745, -3.538124999999807674, 1.026728768593236030 ) ) ;
#1172 = CONICAL_SURFACE ( 'NONE', #7125, 3.749999999999996447, 0.7853981633974476129 ) ;
#1173 = EDGE_CURVE ( 'NONE', #1706, #5891, #11563, .T. ) ;
#1174 = DIRECTION ( 'NONE',  ( -1.000000000000000000, 0.000000000000000000, 0.000000000000000000 ) ) ;
#1175 = CARTESIAN_POINT ( 'NONE',  ( -49.02438362644100067, 99.17411849586700612, -150.4984795835770228 ) ) ;
#1176 = CARTESIAN_POINT ( 'NONE',  ( -13.41835358098578723, 12.39999970914576188, -9.367156043074160721 ) ) ;
#1177 = CARTESIAN_POINT ( 'NONE',  ( -13.41835358098578723, -2.908542394189813650E-07, -11.73358795631400930 ) ) ;
#1178 = CARTESIAN_POINT ( 'NONE',  ( -52.77438362644100067, 99.17411849586700612, -147.9984795835769944 ) ) ;
#1179 = CARTESIAN_POINT ( 'NONE',  ( -4.296789059413591794, -0.4989263220255817921, -0.007758693162678284572 ) ) ;
#1180 = CARTESIAN_POINT ( 'NONE',  ( 22.58164641901421632, -12.40000029085423883, -9.367156043074160721 ) ) ;
#1181 = ADVANCED_FACE ( 'NONE', ( #1910 ), #14700, .F. ) ;
#1182 = CARTESIAN_POINT ( 'NONE',  ( -37.27438362644000591, 104.6741184958670061, -15.85886927678779834 ) ) ;
#1183 = LINE ( 'NONE', #12897, #3792 ) ;
#1184 = VERTEX_POINT ( 'NONE', #12393 ) ;
#1185 = FACE_OUTER_BOUND ( 'NONE', #435, .T. ) ;
#1186 = ADVANCED_FACE ( 'NONE', ( #4239, #585 ), #8893, .T. ) ;
#1187 = ORIENTED_EDGE ( 'NONE', *, *, #9491, .T. ) ;
#1188 = AXIS2_PLACEMENT_3D ( 'NONE', #5400, #14833, #9016 ) ;
#1189 = EDGE_CURVE ( 'NONE', #6732, #7286, #13704, .T. ) ;
#1190 = VERTEX_POINT ( 'NONE', #13851 ) ;
#1191 = CARTESIAN_POINT ( 'NONE',  ( 2.445585954864915479, 0.1562500000001365852, 3.662202016184997522 ) ) ;
#1192 = EDGE_LOOP ( 'NONE', ( #874, #14609, #11340, #2381 ) ) ;
#1193 = CARTESIAN_POINT ( 'NONE',  ( -3.981650243116422683, -0.5617135623731067673, 1.648008353199287290 ) ) ;
#1194 = EDGE_CURVE ( 'NONE', #9060, #4529, #3387, .T. ) ;
#1195 = CARTESIAN_POINT ( 'NONE',  ( -86.77438362644100778, 99.17411849586700612, -182.2484795835770228 ) ) ;
#1196 = FACE_OUTER_BOUND ( 'NONE', #11852, .T. ) ;
#1197 = AXIS2_PLACEMENT_3D ( 'NONE', #622, #3895, #8620 ) ;
#1198 = PLANE ( 'NONE',  #9735 ) ;
#1199 = ADVANCED_FACE ( 'NONE', ( #4087, #8814 ), #3074, .T. ) ;
#1200 = DIRECTION ( 'NONE',  ( -0.000000000000000000, 1.000000000000000000, -0.000000000000000000 ) ) ;
#1201 = VERTEX_POINT ( 'NONE', #12464 ) ;
#1202 = CARTESIAN_POINT ( 'NONE',  ( -58.27438362644001302, 82.17411849586700612, -83.44847958357698303 ) ) ;
#1203 = CARTESIAN_POINT ( 'NONE',  ( 16.59106891544169571, 11.89170417910964872, 0.2558302058915557509 ) ) ;
#1204 = ORIENTED_EDGE ( 'NONE', *, *, #11026, .T. ) ;
#1205 = AXIS2_PLACEMENT_3D ( 'NONE', #290, #11235, #14791 ) ;
#1206 = CARTESIAN_POINT ( 'NONE',  ( -4.500000000000006217, 2.374999999999988454, 0.000000000000000000 ) ) ;
#1207 = CARTESIAN_POINT ( 'NONE',  ( 2.991150664073139342, -3.890625000000195399, 2.452944570972435567 ) ) ;
#1208 = ORIENTED_EDGE ( 'NONE', *, *, #1560, .T. ) ;
#1209 = CYLINDRICAL_SURFACE ( 'NONE', #13169, 8.000000000000007105 ) ;
#1210 = CARTESIAN_POINT ( 'NONE',  ( -86.77438362643999881, 65.17411849586700612, -145.4984795835769944 ) ) ;
#1211 = LINE ( 'NONE', #5970, #14749 ) ;
#1212 = PLANE ( 'NONE',  #10583 ) ;
#1213 = CARTESIAN_POINT ( 'NONE',  ( -69.77438362644001302, 82.17411849586700612, -85.04847958357699156 ) ) ;
#1214 = CARTESIAN_POINT ( 'NONE',  ( -66.41143315690761995, 66.60412428008086749, -83.44847958357698303 ) ) ;
#1215 = CARTESIAN_POINT ( 'NONE',  ( -55.47438362644000165, 65.17411849586700612, -145.4984795835769944 ) ) ;
#1216 = CARTESIAN_POINT ( 'NONE',  ( -72.92551479769302603, 94.57411849586699759, -93.49847958357699440 ) ) ;
#1217 = PLANE ( 'NONE',  #12937 ) ;
#1218 = ORIENTED_EDGE ( 'NONE', *, *, #10001, .F. ) ;
#1219 = CARTESIAN_POINT ( 'NONE',  ( -1.629699455448989389E-14, 8.699999999999999289, 5.655858585055787181E-29 ) ) ;
#1220 = VERTEX_POINT ( 'NONE', #6661 ) ;
#1221 = PLANE ( 'NONE',  #3828 ) ;
#1222 = CARTESIAN_POINT ( 'NONE',  ( 1.740706783794652823, -2.413124999999917808, 3.253752085064650412 ) ) ;
#1223 = ORIENTED_EDGE ( 'NONE', *, *, #2209, .T. ) ;
#1224 = ORIENTED_EDGE ( 'NONE', *, *, #9575, .F. ) ;
#1225 = VERTEX_POINT ( 'NONE', #11371 ) ;
#1226 = PRODUCT_DEFINITION_FORMATION_WITH_SPECIFIED_SOURCE ( 'ANY', '', #2385, .NOT_KNOWN. ) ;
#1227 = CARTESIAN_POINT ( 'NONE',  ( -1.090569219518439548, -4.702338562373102882, 3.599880871716213626 ) ) ;
#1228 = CARTESIAN_POINT ( 'NONE',  ( -30.00000000000000000, -5.000000000000000000, 27.00000000000000000 ) ) ;
#1229 = DIRECTION ( 'NONE',  ( -0.000000000000000000, 1.000000000000000000, 0.000000000000000000 ) ) ;
#1230 = EDGE_CURVE ( 'NONE', #10445, #7422, #3149, .T. ) ;
#1231 = CARTESIAN_POINT ( 'NONE',  ( -9.503456061879928640, -12.00000029085427222, 69.60114695342350899 ) ) ;
#1232 = FACE_OUTER_BOUND ( 'NONE', #12141, .T. ) ;
#1233 = CARTESIAN_POINT ( 'NONE',  ( -86.77438362644001302, 110.1741184958670061, -15.85886927678779834 ) ) ;
#1234 = CARTESIAN_POINT ( 'NONE',  ( 0.001278483876788636883, -4.335000000000164277, 3.435880605283331501 ) ) ;
#1235 = DIRECTION ( 'NONE',  ( -1.000000000000000000, 0.000000000000000000, 0.000000000000000000 ) ) ;
#1236 = ORIENTED_EDGE ( 'NONE', *, *, #10242, .T. ) ;
#1237 = FACE_OUTER_BOUND ( 'NONE', #7306, .T. ) ;
#1238 = ORIENTED_EDGE ( 'NONE', *, *, #4504, .F. ) ;
#1239 = ORIENTED_EDGE ( 'NONE', *, *, #2752, .T. ) ;
#1240 = ORIENTED_EDGE ( 'NONE', *, *, #3079, .T. ) ;
#1241 = CYLINDRICAL_SURFACE ( 'NONE', #11950, 1.999999999999988010 ) ;
#1242 = EDGE_CURVE ( 'NONE', #2988, #13856, #2144, .T. ) ;
#1243 = CARTESIAN_POINT ( 'NONE',  ( 2.928286698324767290, -3.678750000000110987, -1.958188979435658839 ) ) ;
#1244 = DIRECTION ( 'NONE',  ( 0.000000000000000000, 0.000000000000000000, -1.000000000000000000 ) ) ;
#1245 = CARTESIAN_POINT ( 'NONE',  ( 3.163831456873871684, -5.086585887928589678, -1.913743399047732607 ) ) ;
#1246 = LINE ( 'NONE', #4832, #3529 ) ;
#1247 = EDGE_CURVE ( 'NONE', #12468, #4454, #13924, .T. ) ;
#1248 = DIRECTION ( 'NONE',  ( 0.000000000000000000, 0.000000000000000000, -1.000000000000000000 ) ) ;
#1249 = LINE ( 'NONE', #7699, #11092 ) ;
#1250 = CARTESIAN_POINT ( 'NONE',  ( -69.77438362644001302, 82.17411849586700612, -112.9984795835769944 ) ) ;
#1251 = CARTESIAN_POINT ( 'NONE',  ( -84.27438362643998460, 65.17411849586700612, -182.2484795835770228 ) ) ;
#1252 = CARTESIAN_POINT ( 'NONE',  ( -52.77438362644100067, 101.5320169952374414, -147.9984795835769944 ) ) ;
#1253 = CARTESIAN_POINT ( 'NONE',  ( -85.75338362643999801, 66.94254237039483257, -147.9984795835769944 ) ) ;
#1254 = ORIENTED_EDGE ( 'NONE', *, *, #1173, .F. ) ;
#1255 = CYLINDRICAL_SURFACE ( 'NONE', #70, 4.000000000000004441 ) ;
#1256 = ORIENTED_EDGE ( 'NONE', *, *, #12725, .T. ) ;
#1257 = EDGE_LOOP ( 'NONE', ( #13800, #5512, #2573, #2575 ) ) ;
#1258 = EDGE_LOOP ( 'NONE', ( #8908, #11095, #11894 ) ) ;
#1259 = CARTESIAN_POINT ( 'NONE',  ( 4.187874307737824431, -0.04687499999988285065, -1.272022143297006025 ) ) ;
#1260 = ORIENTED_EDGE ( 'NONE', *, *, #8372, .F. ) ;
#1261 = EDGE_CURVE ( 'NONE', #9847, #1912, #11911, .T. ) ;
#1262 = CARTESIAN_POINT ( 'NONE',  ( -4.296821574387140963, -0.4992135623730943328, -3.600545362394707632E-13 ) ) ;
#1263 = AXIS2_PLACEMENT_3D ( 'NONE', #14836, #6645, #722 ) ;
#1264 = CARTESIAN_POINT ( 'NONE',  ( -16.33565937784310762, -0.3156604612129118026, 21.53909249377453250 ) ) ;
#1265 = EDGE_CURVE ( 'NONE', #6718, #14328, #8183, .T. ) ;
#1266 = CARTESIAN_POINT ( 'NONE',  ( 57.41329019055577021, 0.000000000000000000, 95.72362361919107343 ) ) ;
#1267 = AXIS2_PLACEMENT_3D ( 'NONE', #823, #11377, #6737 ) ;
#1268 = DIRECTION ( 'NONE',  ( 1.000000000000000000, 0.000000000000000000, 0.000000000000000000 ) ) ;
#1269 = LINE ( 'NONE', #9488, #14702 ) ;
#1270 = ORIENTED_EDGE ( 'NONE', *, *, #2619, .T. ) ;
#1271 = LINE ( 'NONE', #14150, #5141 ) ;
#1272 = CARTESIAN_POINT ( 'NONE',  ( -86.77438362644100778, 99.17411849586700612, -145.2984795835770058 ) ) ;
#1273 = CIRCLE ( 'NONE', #12437, 2.999999999999999112 ) ;
#1274 = EDGE_CURVE ( 'NONE', #2616, #5168, #11835, .T. ) ;
#1275 = APPLICATION_PROTOCOL_DEFINITION ( 'draft international standard', 'automotive_design', 1998, #4069 ) ;
#1276 = ORIENTED_EDGE ( 'NONE', *, *, #5565, .T. ) ;
#1277 = AXIS2_PLACEMENT_3D ( 'NONE', #954, #12606, #12752 ) ;
#1278 = CARTESIAN_POINT ( 'NONE',  ( -1.775679308629948050, -4.671875000000182077, 3.319983975552966537 ) ) ;
#1279 = ORIENTED_EDGE ( 'NONE', *, *, #2419, .F. ) ;
#1280 = AXIS2_PLACEMENT_3D ( 'NONE', #10048, #1980, #4088 ) ;
#1281 = ADVANCED_FACE ( 'NONE', ( #2208 ), #4540, .F. ) ;
#1282 = CARTESIAN_POINT ( 'NONE',  ( 0.7624512442115692901, -0.8037500000000172840, -3.827857439461599398 ) ) ;
#1283 = LINE ( 'NONE', #9500, #11918 ) ;
#1284 = EDGE_CURVE ( 'NONE', #14787, #6768, #3295, .T. ) ;
#1285 = DIRECTION ( 'NONE',  ( -1.000000000000000000, 0.000000000000000000, 0.000000000000000000 ) ) ;
#1286 = AXIS2_PLACEMENT_3D ( 'NONE', #784, #5541, #10396 ) ;
#1287 = EDGE_CURVE ( 'NONE', #6270, #8008, #30, .T. ) ;
#1288 = CARTESIAN_POINT ( 'NONE',  ( -86.77438362644001302, 99.17411849586700612, -145.4984795835769660 ) ) ;
#1289 = CARTESIAN_POINT ( 'NONE',  ( 14.25000000000000000, -2.500000000000000000, 23.22168783648699986 ) ) ;
#1290 = DIRECTION ( 'NONE',  ( 0.000000000000000000, 1.000000000000000000, 0.000000000000000000 ) ) ;
#1291 = DIRECTION ( 'NONE',  ( 0.000000000000000000, -0.000000000000000000, 1.000000000000000000 ) ) ;
#1292 = VECTOR ( 'NONE', #15054, 1000.000000000000000 ) ;
#1293 = VERTEX_POINT ( 'NONE', #1202 ) ;
#1294 = CARTESIAN_POINT ( 'NONE',  ( -52.77438362644100067, 99.17411849586700612, -182.2484795835770228 ) ) ;
#1295 = CARTESIAN_POINT ( 'NONE',  ( 0.000000000000000000, 0.000000000000000000, 0.000000000000000000 ) ) ;
#1296 = ORIENTED_EDGE ( 'NONE', *, *, #8726, .F. ) ;
#1297 = COLOUR_RGB ( '', 0.09019608, 0.27058824, 0.51372549) ;
#1298 = FACE_OUTER_BOUND ( 'NONE', #1404, .T. ) ;
#1299 = CARTESIAN_POINT ( 'NONE',  ( 1.363531154075422469, -3.397500000000037712, 3.288412936073061399 ) ) ;
#1300 = ORIENTED_EDGE ( 'NONE', *, *, #9712, .F. ) ;
#1301 = EDGE_LOOP ( 'NONE', ( #14048, #2174, #14673, #6484 ) ) ;
#1302 = ORIENTED_EDGE ( 'NONE', *, *, #3096, .T. ) ;
#1303 = AXIS2_PLACEMENT_3D ( 'NONE', #4083, #13475, #7432 ) ;
#1304 = FACE_OUTER_BOUND ( 'NONE', #9267, .T. ) ;
#1305 = LINE ( 'NONE', #10691, #9080 ) ;
#1306 = CARTESIAN_POINT ( 'NONE',  ( -4.330127018922191873, -1.133557105241920558E-14, -1.499999999999999334 ) ) ;
#1307 = CIRCLE ( 'NONE', #9731, 1.250000000000001110 ) ;
#1308 = CARTESIAN_POINT ( 'NONE',  ( 7.511572993685698521E-16, 1.916901515185129432E-30, 4.500000000000000888 ) ) ;
#1309 = FILL_AREA_STYLE ('',( #6070 ) ) ;
#1310 = DIRECTION ( 'NONE',  ( -0.08715574274766053897, 1.511911130105616684E-16, 0.9961946980917454342 ) ) ;
#1311 = CARTESIAN_POINT ( 'NONE',  ( -0.6956252696767697419, -3.303750000000123421, 3.503916970779588969 ) ) ;
#1312 = DIRECTION ( 'NONE',  ( 0.000000000000000000, 0.000000000000000000, -1.000000000000000000 ) ) ;
#1313 = VERTEX_POINT ( 'NONE', #3611 ) ;
#1314 = DIRECTION ( 'NONE',  ( 1.000000000000000000, 0.000000000000000000, -6.982962677686266711E-15 ) ) ;
#1315 = AXIS2_PLACEMENT_3D ( 'NONE', #14886, #4276, #9004 ) ;
#1316 = EDGE_LOOP ( 'NONE', ( #6456, #4036, #931, #1168 ) ) ;
#1317 = EDGE_LOOP ( 'NONE', ( #5440, #5241, #14278, #9761 ) ) ;
#1318 = ORIENTED_EDGE ( 'NONE', *, *, #12388, .T. ) ;
#1319 = VECTOR ( 'NONE', #11873, 1000.000000000000000 ) ;
#1320 = DIRECTION ( 'NONE',  ( 0.000000000000000000, 0.000000000000000000, -1.000000000000000000 ) ) ;
#1321 = CARTESIAN_POINT ( 'NONE',  ( 3.273328345814555007, -3.522500000000126974, 1.356842221127619874 ) ) ;
#1322 = CARTESIAN_POINT ( 'NONE',  ( 15.50000000000000000, -5.000000000000000000, 22.50000000000000000 ) ) ;
#1323 = PLANE ( 'NONE',  #4014 ) ;
#1324 = AXIS2_PLACEMENT_3D ( 'NONE', #14681, #1434, #256 ) ;
#1325 = DIRECTION ( 'NONE',  ( 0.000000000000000000, 1.000000000000000000, 0.000000000000000000 ) ) ;
#1326 = VECTOR ( 'NONE', #14944, 1000.000000000000000 ) ;
#1327 = CARTESIAN_POINT ( 'NONE',  ( -12.81835358098578403, 11.99999970914575798, -0.3335879563140091153 ) ) ;
#1328 = CARTESIAN_POINT ( 'NONE',  ( -86.77438362644001302, 59.67411849586700612, -152.4984795835769944 ) ) ;
#1329 = CARTESIAN_POINT ( 'NONE',  ( -90.52438362643999881, 65.17411849586700612, -150.4984795835770228 ) ) ;
#1330 = CARTESIAN_POINT ( 'NONE',  ( 10.10406781373725771, -11.00000029085427045, 69.08979243323352648 ) ) ;
#1331 = CARTESIAN_POINT ( 'NONE',  ( -3.081487911019577365E-30, 0.000000000000000000, 0.000000000000000000 ) ) ;
#1332 = CARTESIAN_POINT ( 'NONE',  ( -14.25000000000000000, -2.500000000000000000, 23.22168783648699986 ) ) ;
#1333 = VERTEX_POINT ( 'NONE', #2135 ) ;
#1334 = PLANE ( 'NONE',  #1426 ) ;
#1335 = EDGE_CURVE ( 'NONE', #14415, #13870, #660, .T. ) ;
#1336 = ORIENTED_EDGE ( 'NONE', *, *, #3538, .F. ) ;
#1337 = ORIENTED_EDGE ( 'NONE', *, *, #9200, .T. ) ;
#1338 = ORIENTED_EDGE ( 'NONE', *, *, #14365, .T. ) ;
#1339 = CARTESIAN_POINT ( 'NONE',  ( 1.581646419014216542, 11.99999970914575798, -0.3335879563140091153 ) ) ;
#1340 = CLOSED_SHELL ( 'NONE', ( #1484, #14239, #7741, #10570, #14326, #4894, #5553, #4994, #9912, #11153, #4510, #6147, #11998, #6486 ) ) ;
#1341 = CIRCLE ( 'NONE', #1600, 10.20000000000000107 ) ;
#1342 = EDGE_CURVE ( 'NONE', #6229, #10656, #6534, .T. ) ;
#1343 = AXIS2_PLACEMENT_3D ( 'NONE', #10603, #3548, #2382 ) ;
#1344 = CARTESIAN_POINT ( 'NONE',  ( -4.103321639749550442, 0.4374999999999862332, 1.698361598734861477 ) ) ;
#1345 = ORIENTED_EDGE ( 'NONE', *, *, #5839, .T. ) ;
#1346 = CARTESIAN_POINT ( 'NONE',  ( 1.240811975207549933, -0.7960885623730461491, 4.094338395617355353 ) ) ;
#1347 = CARTESIAN_POINT ( 'NONE',  ( 40.52020888806953991, -24.00000000000000000, 6.000000000000000000 ) ) ;
#1348 = CARTESIAN_POINT ( 'NONE',  ( -50.73238362643999722, 63.99516924618178848, -147.9984795835769944 ) ) ;
#1349 = CARTESIAN_POINT ( 'NONE',  ( -35.27438362644000591, 0.000000000000000000, 0.000000000000000000 ) ) ;
#1350 = AXIS2_PLACEMENT_3D ( 'NONE', #14641, #7534, #8753 ) ;
#1351 = AXIS2_PLACEMENT_3D ( 'NONE', #14097, #4713, #8040 ) ;
#1352 = DIRECTION ( 'NONE',  ( 0.000000000000000000, 0.000000000000000000, -1.000000000000000000 ) ) ;
#1353 = ORIENTED_EDGE ( 'NONE', *, *, #4149, .F. ) ;
#1354 = EDGE_CURVE ( 'NONE', #4630, #15067, #8348, .T. ) ;
#1355 = CYLINDRICAL_SURFACE ( 'NONE', #8095, 4.500000000000003553 ) ;
#1356 = EDGE_CURVE ( 'NONE', #12262, #8420, #14084, .T. ) ;
#1357 = DIRECTION ( 'NONE',  ( -1.747085166004344019E-15, 1.000000000000000000, -0.000000000000000000 ) ) ;
#1358 = ORIENTED_EDGE ( 'NONE', *, *, #3640, .T. ) ;
#1359 = EDGE_CURVE ( 'NONE', #3822, #12945, #13090, .T. ) ;
#1360 = CARTESIAN_POINT ( 'NONE',  ( 3.783699349552338997, -3.968750000000262013, 0.7536532579988950431 ) ) ;
#1361 = ORIENTED_EDGE ( 'NONE', *, *, #15071, .T. ) ;
#1362 = VECTOR ( 'NONE', #3810, 1000.000000000000000 ) ;
#1363 = VECTOR ( 'NONE', #4751, 1000.000000000000000 ) ;
#1364 = FACE_OUTER_BOUND ( 'NONE', #13451, .T. ) ;
#1365 = CARTESIAN_POINT ( 'NONE',  ( -69.77438362644001302, 82.17411849586700612, -81.84847958357698872 ) ) ;
#1366 = EDGE_CURVE ( 'NONE', #12409, #2967, #15008, .T. ) ;
#1367 = ADVANCED_FACE ( 'NONE', ( #4701 ), #5720, .T. ) ;
#1368 = CARTESIAN_POINT ( 'NONE',  ( 14.25000000000000000, -2.500000000000000000, 21.77831216351300014 ) ) ;
#1369 = LINE ( 'NONE', #14320, #3433 ) ;
#1370 = PLANE ( 'NONE',  #9719 ) ;
#1371 = DIRECTION ( 'NONE',  ( 0.000000000000000000, 0.000000000000000000, 1.000000000000000000 ) ) ;
#1372 = DIRECTION ( 'NONE',  ( -1.000000000000000000, -1.682335022489801357E-15, 0.000000000000000000 ) ) ;
#1373 = EDGE_CURVE ( 'NONE', #9101, #11935, #1271, .T. ) ;
#1374 = CARTESIAN_POINT ( 'NONE',  ( 11.02010870769206541, -85.69524470659703752, 70.09311034953161368 ) ) ;
#1375 = VECTOR ( 'NONE', #658, 1000.000000000000000 ) ;
#1376 = ORIENTED_EDGE ( 'NONE', *, *, #9420, .T. ) ;
#1377 = CIRCLE ( 'NONE', #3620, 2.750000000000002665 ) ;
#1378 = CYLINDRICAL_SURFACE ( 'NONE', #12228, 4.249999999999996447 ) ;
#1379 = CARTESIAN_POINT ( 'NONE',  ( 16.96309080958207360, 12.51006470759389799, 57.31273383969018198 ) ) ;
#1380 = VERTEX_POINT ( 'NONE', #4463 ) ;
#1381 = ADVANCED_FACE ( 'NONE', ( #6882 ), #3526, .F. ) ;
#1382 = CARTESIAN_POINT ( 'NONE',  ( -86.77438362644001302, 65.17411849586700612, -145.4984795835769660 ) ) ;
#1383 = ADVANCED_FACE ( 'NONE', ( #3380 ), #12847, .F. ) ;
#1384 = CARTESIAN_POINT ( 'NONE',  ( 2.024885806073562389, -2.741249999999974207, -3.032875982375833335 ) ) ;
#1385 = ORIENTED_EDGE ( 'NONE', *, *, #9354, .T. ) ;
#1386 = VERTEX_POINT ( 'NONE', #1589 ) ;
#1387 = ORIENTED_EDGE ( 'NONE', *, *, #1161, .T. ) ;
#1388 = AXIS2_PLACEMENT_3D ( 'NONE', #1252, #10721, #2571 ) ;
#1389 = CARTESIAN_POINT ( 'NONE',  ( -52.77438362643999881, 65.17411849586700612, -150.4984795835770228 ) ) ;
#1390 = AXIS2_PLACEMENT_3D ( 'NONE', #5956, #5789, #10653 ) ;
#1391 = ADVANCED_FACE ( 'NONE', ( #7342, #6036 ), #7420, .T. ) ;
#1392 = VECTOR ( 'NONE', #2531, 1000.000000000000000 ) ;
#1393 = CARTESIAN_POINT ( 'NONE',  ( -35.58670980944424400, 5.000000000000000000, 129.5095611191910621 ) ) ;
#1394 = CARTESIAN_POINT ( 'NONE',  ( -15.50000000000000000, -5.000000000000000000, 19.00000000000000000 ) ) ;
#1395 = DIRECTION ( 'NONE',  ( -1.000000000000000000, 0.000000000000000000, -0.000000000000000000 ) ) ;
#1396 = CARTESIAN_POINT ( 'NONE',  ( 10.10406781373725948, -11.00000029085427933, 69.08979243323352648 ) ) ;
#1397 = LINE ( 'NONE', #7454, #10039 ) ;
#1398 = EDGE_CURVE ( 'NONE', #8134, #15237, #9879, .T. ) ;
#1399 = CARTESIAN_POINT ( 'NONE',  ( 3.109021928378527200, -3.663124999999927578, -1.660781358202984448 ) ) ;
#1400 = DIRECTION ( 'NONE',  ( -2.065146995210485003E-17, -4.130293990420970006E-17, -1.000000000000000000 ) ) ;
#1401 = VERTEX_POINT ( 'NONE', #5006 ) ;
#1402 = CARTESIAN_POINT ( 'NONE',  ( -86.77438362643999881, 65.17411849586700612, -145.2984795835770058 ) ) ;
#1403 = VECTOR ( 'NONE', #11031, 1000.000000000000000 ) ;
#1404 = EDGE_LOOP ( 'NONE', ( #10933, #10528, #6124, #1385 ) ) ;
#1405 = VERTEX_POINT ( 'NONE', #12142 ) ;
#1406 = VERTEX_POINT ( 'NONE', #7262 ) ;
#1407 = VECTOR ( 'NONE', #2415, 1000.000000000000000 ) ;
#1408 = VERTEX_POINT ( 'NONE', #5169 ) ;
#1409 = DIRECTION ( 'NONE',  ( 1.000000000000000000, 0.000000000000000000, 0.000000000000000000 ) ) ;
#1410 = CARTESIAN_POINT ( 'NONE',  ( 0.3573659033054957801, -2.819374999999921805, -3.618812876704415427 ) ) ;
#1411 = DIRECTION ( 'NONE',  ( 0.000000000000000000, 0.000000000000000000, -1.000000000000000000 ) ) ;
#1412 = CIRCLE ( 'NONE', #10066, 3.968749999999992895 ) ;
#1413 = FACE_OUTER_BOUND ( 'NONE', #9244, .T. ) ;
#1414 = FACE_BOUND ( 'NONE', #12531, .T. ) ;
#1415 = CARTESIAN_POINT ( 'NONE',  ( -52.77438362644100067, 99.17411849586700612, -182.2484795835770228 ) ) ;
#1416 = LINE ( 'NONE', #9, #5657 ) ;
#1417 = DIRECTION ( 'NONE',  ( 0.08715574274766176022, 4.320305823558445788E-16, -0.9961946980917453232 ) ) ;
#1418 = FACE_OUTER_BOUND ( 'NONE', #5044, .T. ) ;
#1419 = DIRECTION ( 'NONE',  ( 2.551930889570659960E-15, -1.000000000000000000, -0.000000000000000000 ) ) ;
#1420 = LINE ( 'NONE', #14435, #807 ) ;
#1421 = VERTEX_POINT ( 'NONE', #107 ) ;
#1422 = CARTESIAN_POINT ( 'NONE',  ( 16.50208930436313892, -11.93241838496953910, 0.2532233872428652499 ) ) ;
#1423 = ORIENTED_EDGE ( 'NONE', *, *, #1112, .F. ) ;
#1424 = ORIENTED_EDGE ( 'NONE', *, *, #4905, .F. ) ;
#1425 = CARTESIAN_POINT ( 'NONE',  ( 15.50000000000000000, -0.2000000000000000111, 19.19999999702029925 ) ) ;
#1426 = AXIS2_PLACEMENT_3D ( 'NONE', #9631, #6324, #7323 ) ;
#1427 = VECTOR ( 'NONE', #13016, 1000.000000000000000 ) ;
#1428 = CARTESIAN_POINT ( 'NONE',  ( 10.10406781373725771, -11.00000029085428110, 70.08979243323352648 ) ) ;
#1429 = CARTESIAN_POINT ( 'NONE',  ( -3.700822939793764643, -1.421088562373072239, -1.976411301434599865 ) ) ;
#1430 = DIRECTION ( 'NONE',  ( -1.747085166004344019E-15, 1.000000000000000000, -0.000000000000000000 ) ) ;
#1431 = DIRECTION ( 'NONE',  ( 0.000000000000000000, 0.000000000000000000, -1.000000000000000000 ) ) ;
#1432 = LINE ( 'NONE', #3911, #10285 ) ;
#1433 =( BOUNDED_CURVE ( )  B_SPLINE_CURVE ( 3, ( #9933, #12277, #5531, #1651 ),
 .UNSPECIFIED., .F., .T. ) 
 B_SPLINE_CURVE_WITH_KNOTS ( ( 4, 4 ),
 ( 4.336808689942018229E-16, 1.570796326794896780 ),
 .UNSPECIFIED. ) 
 CURVE ( )  GEOMETRIC_REPRESENTATION_ITEM ( )  RATIONAL_B_SPLINE_CURVE ( ( 1.000000000000000000, 0.8047378541243650485, 0.8047378541243650485, 1.000000000000000000 ) ) 
 REPRESENTATION_ITEM ( '' )  );
#1434 = DIRECTION ( 'NONE',  ( 0.000000000000000000, -1.000000000000000000, -0.000000000000000000 ) ) ;
#1435 = EDGE_CURVE ( 'NONE', #15063, #11245, #4857, .T. ) ;
#1436 = VECTOR ( 'NONE', #7493, 1000.000000000000000 ) ;
#1437 = DIRECTION ( 'NONE',  ( 0.000000000000000000, 0.000000000000000000, -1.000000000000000000 ) ) ;
#1438 = ORIENTED_EDGE ( 'NONE', *, *, #8297, .F. ) ;
#1439 = DIRECTION ( 'NONE',  ( 0.000000000000000000, 1.000000000000000000, 0.000000000000000000 ) ) ;
#1440 = APPLICATION_PROTOCOL_DEFINITION ( 'draft international standard', 'automotive_design', 1998, #5667 ) ;
#1441 = ORIENTED_EDGE ( 'NONE', *, *, #862, .T. ) ;
#1442 = CARTESIAN_POINT ( 'NONE',  ( -3.466918327573330849, -3.421874999999993339, -1.851480974780293387 ) ) ;
#1443 = EDGE_LOOP ( 'NONE', ( #933, #5709, #3137, #8529 ) ) ;
#1444 = CIRCLE ( 'NONE', #6664, 4.500000000000003553 ) ;
#1445 = CARTESIAN_POINT ( 'NONE',  ( -69.77438362644001302, 82.17411849586700612, -29.37106258560738681 ) ) ;
#1446 = ADVANCED_FACE ( 'NONE', ( #14607 ), #11315, .T. ) ;
#1447 = CARTESIAN_POINT ( 'NONE',  ( -1.967370292840699531, -5.340790585608573338, 2.765304479937676696 ) ) ;
#1448 = PLANE ( 'NONE',  #10022 ) ;
#1449 = EDGE_CURVE ( 'NONE', #7901, #10851, #6635, .T. ) ;
#1450 = DIRECTION ( 'NONE',  ( -2.551930889570660354E-15, 1.000000000000000000, 0.000000000000000000 ) ) ;
#1451 = DIRECTION ( 'NONE',  ( -1.287488025362404182E-15, -1.000000000000000000, 0.000000000000000000 ) ) ;
#1452 = CARTESIAN_POINT ( 'NONE',  ( -88.81638362644100937, 97.99516924618178848, -150.4984795835770228 ) ) ;
#1453 = LINE ( 'NONE', #1525, #15254 ) ;
#1454 = DIRECTION ( 'NONE',  ( 0.9961946980917453232, -3.779777825264105188E-17, 0.08715574274766176022 ) ) ;
#1455 = CIRCLE ( 'NONE', #3194, 2.042000000000002036 ) ;
#1456 = ORIENTED_EDGE ( 'NONE', *, *, #11326, .T. ) ;
#1457 = CARTESIAN_POINT ( 'NONE',  ( -46.58670980944423690, 5.000000000000000000, 89.50956111919107627 ) ) ;
#1458 = SHAPE_REPRESENTATION_RELATIONSHIP ( 'NONE' , 'NONE' ,  #6613, #9048 ) ;
#1459 = VERTEX_POINT ( 'NONE', #7579 ) ;
#1460 = DIRECTION ( 'NONE',  ( -6.860497997771531562E-15, -6.464231808267455010E-30, -1.000000000000000000 ) ) ;
#1461 = CARTESIAN_POINT ( 'NONE',  ( -0.001340710925747427232, -2.834999999999994635, -3.634308738048292131 ) ) ;
#1462 = ORIENTED_EDGE ( 'NONE', *, *, #8859, .F. ) ;
#1463 = ORIENTED_EDGE ( 'NONE', *, *, #12940, .F. ) ;
#1464 = ORIENTED_EDGE ( 'NONE', *, *, #3572, .T. ) ;
#1465 = CARTESIAN_POINT ( 'NONE',  ( 68.41329019055577021, 5.000000000000000000, 135.5095611191910621 ) ) ;
#1466 = EDGE_CURVE ( 'NONE', #4666, #6139, #13389, .T. ) ;
#1467 = CIRCLE ( 'NONE', #10121, 3.499999999999999556 ) ;
#1468 = CARTESIAN_POINT ( 'NONE',  ( -52.77438362643999881, 65.17411849586700612, -147.9984795835769944 ) ) ;
#1469 = LINE ( 'NONE', #3713, #11498 ) ;
#1470 = EDGE_CURVE ( 'NONE', #14932, #2765, #1412, .T. ) ;
#1471 = ADVANCED_FACE ( 'NONE', ( #2828 ), #14378, .T. ) ;
#1472 = DIRECTION ( 'NONE',  ( 0.000000000000000000, 0.000000000000000000, -1.000000000000000000 ) ) ;
#1473 = DIRECTION ( 'NONE',  ( 0.000000000000000000, 0.000000000000000000, 1.000000000000000000 ) ) ;
#1474 = DIRECTION ( 'NONE',  ( 0.000000000000000000, 0.000000000000000000, 1.000000000000000000 ) ) ;
#1475 = CYLINDRICAL_SURFACE ( 'NONE', #1350, 2.999999999999999112 ) ;
#1476 = ORIENTED_EDGE ( 'NONE', *, *, #3651, .F. ) ;
#1477 = CARTESIAN_POINT ( 'NONE',  ( -57.27438362644000591, 99.17411849586700612, -79.59847958357700293 ) ) ;
#1478 = ORIENTED_EDGE ( 'NONE', *, *, #4198, .F. ) ;
#1479 = ADVANCED_FACE ( 'NONE', ( #2743 ), #8837, .T. ) ;
#1480 = ORIENTED_EDGE ( 'NONE', *, *, #8476, .F. ) ;
#1481 = VERTEX_POINT ( 'NONE', #13233 ) ;
#1482 = ORIENTED_EDGE ( 'NONE', *, *, #10428, .T. ) ;
#1483 = CARTESIAN_POINT ( 'NONE',  ( -76.48108760497456160, 68.65632084656354550, -83.44847958357698303 ) ) ;
#1484 = ADVANCED_FACE ( 'NONE', ( #8417 ), #13159, .F. ) ;
#1485 = DIRECTION ( 'NONE',  ( 0.000000000000000000, 1.000000000000000000, 0.000000000000000000 ) ) ;
#1486 = CARTESIAN_POINT ( 'NONE',  ( -1.859859099471618649, -3.328125000000058620, -3.476502332403788476 ) ) ;
#1487 = DIRECTION ( 'NONE',  ( 1.000000000000000000, 0.000000000000000000, 0.000000000000000000 ) ) ;
#1488 = LINE ( 'NONE', #2882, #2375 ) ;
#1489 = EDGE_CURVE ( 'NONE', #8820, #10769, #12802, .T. ) ;
#1490 = ORIENTED_EDGE ( 'NONE', *, *, #6678, .F. ) ;
#1491 = ADVANCED_FACE ( 'NONE', ( #10826 ), #1355, .F. ) ;
#1492 = DIRECTION ( 'NONE',  ( 1.000000000000000000, 0.000000000000000000, 0.000000000000000000 ) ) ;
#1493 = CARTESIAN_POINT ( 'NONE',  ( -80.52077156573417938, 59.67411849586701322, -79.59847958357700293 ) ) ;
#1494 = DIRECTION ( 'NONE',  ( 0.5000000000000003331, 0.8660254037844384856, 0.000000000000000000 ) ) ;
#1495 = DIRECTION ( 'NONE',  ( 0.3479852726768751237, 0.000000000000000000, -0.9375000000000004441 ) ) ;
#1496 = CARTESIAN_POINT ( 'NONE',  ( -69.77438362643999881, 89.17411849586052597, -43.99847958364157563 ) ) ;
#1497 = VERTEX_POINT ( 'NONE', #10976 ) ;
#1498 = CARTESIAN_POINT ( 'NONE',  ( -88.81638362644000040, 63.99516924618178848, -150.4984795835770228 ) ) ;
#1499 = ORIENTED_EDGE ( 'NONE', *, *, #5654, .F. ) ;
#1500 = ORIENTED_EDGE ( 'NONE', *, *, #4502, .F. ) ;
#1501 = CARTESIAN_POINT ( 'NONE',  ( -2.968563080203957760, -6.022500000000311715, -1.228311040920463615 ) ) ;
#1502 = LINE ( 'NONE', #5308, #8712 ) ;
#1503 = CARTESIAN_POINT ( 'NONE',  ( 3.523678346781135229, -1.092963562373023167, -2.356287093288357060 ) ) ;
#1504 = DIRECTION ( 'NONE',  ( 0.000000000000000000, 0.000000000000000000, -1.000000000000000000 ) ) ;
#1505 = DIRECTION ( 'NONE',  ( -1.000000000000000000, 0.000000000000000000, 0.000000000000000000 ) ) ;
#1506 = DIRECTION ( 'NONE',  ( -6.982962677686266711E-15, -6.579622859988665673E-30, -1.000000000000000000 ) ) ;
#1507 = LINE ( 'NONE', #5083, #2323 ) ;
#1508 = DIRECTION ( 'NONE',  ( 0.000000000000000000, 0.000000000000000000, -1.000000000000000000 ) ) ;
#1509 = ORIENTED_EDGE ( 'NONE', *, *, #6408, .T. ) ;
#1510 = DIRECTION ( 'NONE',  ( 0.000000000000000000, 0.000000000000000000, 1.000000000000000000 ) ) ;
#1511 = ORIENTED_EDGE ( 'NONE', *, *, #2723, .F. ) ;
#1512 = VECTOR ( 'NONE', #13696, 1000.000000000000000 ) ;
#1513 = CARTESIAN_POINT ( 'NONE',  ( -3.711107677420292905, -4.531250000000010658, 0.7371803430742600582 ) ) ;
#1514 = ORIENTED_EDGE ( 'NONE', *, *, #993, .T. ) ;
#1515 = CARTESIAN_POINT ( 'NONE',  ( 2.057266006166119432, -5.155463562373004294, -3.077188522048795338 ) ) ;
#1516 = VECTOR ( 'NONE', #12476, 1000.000000000000000 ) ;
#1517 = CARTESIAN_POINT ( 'NONE',  ( -0.7612222386588485268, -0.8662499999999671019, -3.819631723157196568 ) ) ;
#1518 = CARTESIAN_POINT ( 'NONE',  ( -4.522482571421199360, 11.99999970914574021, 70.03692566716181034 ) ) ;
#1519 = CARTESIAN_POINT ( 'NONE',  ( -15.50000000000000000, -0.4000000000000000222, -19.00000000000000355 ) ) ;
#1520 = CARTESIAN_POINT ( 'NONE',  ( -61.64938362644000591, 82.17411849586700612, -150.4984795835769944 ) ) ;
#1521 = VECTOR ( 'NONE', #9793, 1000.000000000000000 ) ;
#1522 = PLANE ( 'NONE',  #10361 ) ;
#1523 = CARTESIAN_POINT ( 'NONE',  ( 3.500468167958952659, -5.241858618441043838, 0.2938655770740091211 ) ) ;
#1524 = CARTESIAN_POINT ( 'NONE',  ( -50.02438362644000591, 99.17411849586700612, -86.49847958357699440 ) ) ;
#1525 = CARTESIAN_POINT ( 'NONE',  ( 17.12895037488186389, -12.00000029085424025, 0.2687305842673423095 ) ) ;
#1526 = AXIS2_PLACEMENT_3D ( 'NONE', #6553, #1657, #14598 ) ;
#1527 = ORIENTED_EDGE ( 'NONE', *, *, #15018, .T. ) ;
#1528 = VERTEX_POINT ( 'NONE', #189 ) ;
#1529 = EDGE_CURVE ( 'NONE', #12869, #11817, #5089, .T. ) ;
#1530 = ORIENTED_EDGE ( 'NONE', *, *, #6128, .T. ) ;
#1531 = CARTESIAN_POINT ( 'NONE',  ( -69.77438362644001302, 79.67411849586700612, -67.69567958357700377 ) ) ;
#1532 = CARTESIAN_POINT ( 'NONE',  ( 2.605880849243188191, -2.459999999999848086, 2.603962797083296365 ) ) ;
#1533 = VERTEX_POINT ( 'NONE', #3056 ) ;
#1534 = ORIENTED_EDGE ( 'NONE', *, *, #15085, .T. ) ;
#1535 = EDGE_CURVE ( 'NONE', #4454, #9228, #7870, .T. ) ;
#1536 = AXIS2_PLACEMENT_3D ( 'NONE', #13043, #7148, #11869 ) ;
#1537 = DIRECTION ( 'NONE',  ( 0.000000000000000000, 0.000000000000000000, -1.000000000000000000 ) ) ;
#1538 = AXIS2_PLACEMENT_3D ( 'NONE', #1295, #4881, #8365 ) ;
#1539 = DIRECTION ( 'NONE',  ( 0.000000000000000000, 1.000000000000000000, 0.000000000000000000 ) ) ;
#1540 = AXIS2_PLACEMENT_3D ( 'NONE', #14942, #4334, #13798 ) ;
#1541 = DIRECTION ( 'NONE',  ( 0.000000000000000000, 0.000000000000000000, 1.000000000000000000 ) ) ;
#1542 = CARTESIAN_POINT ( 'NONE',  ( -1.552469261541196355, -0.4995676945082632159, -3.889349939136176548 ) ) ;
#1543 = DIRECTION ( 'NONE',  ( 0.000000000000000000, -1.000000000000000000, 0.000000000000000000 ) ) ;
#1544 = CYLINDRICAL_SURFACE ( 'NONE', #15213, 8.050000000000000711 ) ;
#1545 = ORIENTED_EDGE ( 'NONE', *, *, #10949, .F. ) ;
#1546 = DIRECTION ( 'NONE',  ( -1.000000000000000000, 0.000000000000000000, 0.000000000000000000 ) ) ;
#1547 = ADVANCED_FACE ( 'NONE', ( #12529 ), #1893, .F. ) ;
#1548 = ORIENTED_EDGE ( 'NONE', *, *, #980, .F. ) ;
#1549 = ORIENTED_EDGE ( 'NONE', *, *, #14757, .F. ) ;
#1550 = VERTEX_POINT ( 'NONE', #11199 ) ;
#1551 = VERTEX_POINT ( 'NONE', #649 ) ;
#1552 = AXIS2_PLACEMENT_3D ( 'NONE', #5721, #8030, #9413 ) ;
#1553 = EDGE_CURVE ( 'NONE', #15023, #5866, #5990, .T. ) ;
#1554 = LINE ( 'NONE', #9921, #3084 ) ;
#1555 = CARTESIAN_POINT ( 'NONE',  ( 3.059130242547580814, -2.491250000000117204, 2.045191655759024396 ) ) ;
#1556 = VECTOR ( 'NONE', #12230, 1000.000000000000000 ) ;
#1557 = CARTESIAN_POINT ( 'NONE',  ( -1.106373576938931125, -4.296874999999863221, -3.650653549769442119 ) ) ;
#1558 = PLANE ( 'NONE',  #8987 ) ;
#1559 = CARTESIAN_POINT ( 'NONE',  ( 16.33757311576526305, -0.3152598339554795182, 21.54019739087904384 ) ) ;
#1560 = EDGE_CURVE ( 'NONE', #9136, #8597, #10173, .T. ) ;
#1561 = DIRECTION ( 'NONE',  ( 0.000000000000000000, 0.000000000000000000, 1.000000000000000000 ) ) ;
#1562 = FACE_BOUND ( 'NONE', #6813, .T. ) ;
#1563 = DIRECTION ( 'NONE',  ( 0.000000000000000000, 0.000000000000000000, -1.000000000000000000 ) ) ;
#1564 = AXIS2_PLACEMENT_3D ( 'NONE', #6538, #477, #5212 ) ;
#1565 = DIRECTION ( 'NONE',  ( -0.000000000000000000, 1.000000000000000000, -0.000000000000000000 ) ) ;
#1566 = AXIS2_PLACEMENT_3D ( 'NONE', #4357, #8153, #15274 ) ;
#1567 = DIRECTION ( 'NONE',  ( 0.000000000000000000, 0.000000000000000000, -1.000000000000000000 ) ) ;
#1568 = ORIENTED_EDGE ( 'NONE', *, *, #8174, .F. ) ;
#1569 = CARTESIAN_POINT ( 'NONE',  ( 16.31427926918344085, -11.98694815350135379, 0.2637688259798897095 ) ) ;
#1570 = EDGE_CURVE ( 'NONE', #3974, #1792, #10312, .T. ) ;
#1571 = ORIENTED_EDGE ( 'NONE', *, *, #45, .T. ) ;
#1572 = VECTOR ( 'NONE', #13214, 1000.000000000000000 ) ;
#1573 = ORIENTED_EDGE ( 'NONE', *, *, #6520, .F. ) ;
#1574 = VERTEX_POINT ( 'NONE', #12604 ) ;
#1575 = CARTESIAN_POINT ( 'NONE',  ( -0.001216256839607805784, -5.834999999999983977, -3.237452472516330282 ) ) ;
#1576 = EDGE_CURVE ( 'NONE', #6229, #7479, #5434, .T. ) ;
#1577 = CARTESIAN_POINT ( 'NONE',  ( 0.000000000000000000, 0.000000000000000000, 0.000000000000000000 ) ) ;
#1578 = ADVANCED_FACE ( 'NONE', ( #13617 ), #3136, .F. ) ;
#1579 = CIRCLE ( 'NONE', #11228, 6.999999999974082954 ) ;
#1580 = CARTESIAN_POINT ( 'NONE',  ( -2.933994605034232706, -5.163125000000027498, 1.567297863280144865 ) ) ;
#1581 = DIRECTION ( 'NONE',  ( -1.000000000000000000, 0.000000000000000000, 0.000000000000000000 ) ) ;
#1582 = CARTESIAN_POINT ( 'NONE',  ( -57.27438362644000591, 65.17411849586700612, -145.4984795835769660 ) ) ;
#1583 = CARTESIAN_POINT ( 'NONE',  ( -13.41835358098578723, 11.99999970914576330, -14.13358795631400611 ) ) ;
#1584 = VECTOR ( 'NONE', #13522, 1000.000000000000000 ) ;
#1585 = CARTESIAN_POINT ( 'NONE',  ( -69.77438362644001302, 82.17411849586700612, -79.49847958357700861 ) ) ;
#1586 = DIRECTION ( 'NONE',  ( 0.000000000000000000, 0.000000000000000000, -1.000000000000000000 ) ) ;
#1587 = CARTESIAN_POINT ( 'NONE',  ( 0.000000000000000000, 0.000000000000000000, 6.000000000000000000 ) ) ;
#1588 = VERTEX_POINT ( 'NONE', #11428 ) ;
#1589 = CARTESIAN_POINT ( 'NONE',  ( 1.682902201845278611, -5.420849775684215999, 2.811263474311217259 ) ) ;
#1590 = CIRCLE ( 'NONE', #15189, 16.06499999999999773 ) ;
#1591 = AXIS2_PLACEMENT_3D ( 'NONE', #4880, #4950, #11853 ) ;
#1592 = ADVANCED_FACE ( 'NONE', ( #7656 ), #3208, .F. ) ;
#1593 = ORIENTED_EDGE ( 'NONE', *, *, #4513, .F. ) ;
#1594 = LINE ( 'NONE', #14688, #2872 ) ;
#1595 = CARTESIAN_POINT ( 'NONE',  ( -0.7951559085591690668, -2.281249999999988010, -4.003048974988245412 ) ) ;
#1596 = ORIENTED_EDGE ( 'NONE', *, *, #3761, .T. ) ;
#1597 = CARTESIAN_POINT ( 'NONE',  ( -3.903921151840624493, -3.483588562373245878, -0.3830646067732271787 ) ) ;
#1598 = AXIS2_PLACEMENT_3D ( 'NONE', #279, #13111, #10771 ) ;
#1599 = DIRECTION ( 'NONE',  ( 0.8660254037844383745, -0.5000000000000003331, 0.000000000000000000 ) ) ;
#1600 = AXIS2_PLACEMENT_3D ( 'NONE', #3479, #3643, #10613 ) ;
#1601 = VECTOR ( 'NONE', #2527, 1000.000000000000000 ) ;
#1602 = CARTESIAN_POINT ( 'NONE',  ( 17.18164641901421419, -11.40000029085424238, 0.2664120436859911956 ) ) ;
#1603 = PLANE ( 'NONE',  #5084 ) ;
#1604 = LINE ( 'NONE', #11213, #2951 ) ;
#1605 = PLANE ( 'NONE',  #3535 ) ;
#1606 = CARTESIAN_POINT ( 'NONE',  ( -82.27438362643999881, 99.17411849586700612, -79.59847958357700293 ) ) ;
#1607 = LINE ( 'NONE', #5184, #9066 ) ;
#1608 = ORIENTED_EDGE ( 'NONE', *, *, #3942, .F. ) ;
#1609 =( NAMED_UNIT ( * ) PLANE_ANGLE_UNIT ( ) SI_UNIT ( $, .RADIAN. ) );
#1610 = EDGE_LOOP ( 'NONE', ( #8334, #14233 ) ) ;
#1611 = DIRECTION ( 'NONE',  ( 0.000000000000000000, 0.000000000000000000, -1.000000000000000000 ) ) ;
#1612 = CARTESIAN_POINT ( 'NONE',  ( 2.674095735623996273, -1.709999999999972209, -2.676057788957755701 ) ) ;
#1613 = ORIENTED_EDGE ( 'NONE', *, *, #3658, .F. ) ;
#1614 = AXIS2_PLACEMENT_3D ( 'NONE', #4354, #928, #6764 ) ;
#1615 = PLANE ( 'NONE',  #3743 ) ;
#1616 = CARTESIAN_POINT ( 'NONE',  ( -0.7374914331583092286, -5.180749959738387922, -3.517645758868249040 ) ) ;
#1617 = DIRECTION ( 'NONE',  ( 1.000000000000000000, 0.000000000000000000, 0.000000000000000000 ) ) ;
#1618 = VECTOR ( 'NONE', #7431, 1000.000000000000000 ) ;
#1619 = CARTESIAN_POINT ( 'NONE',  ( -12.81835358098578403, -12.00000029085423670, -11.73358795631400930 ) ) ;
#1620 = PLANE ( 'NONE',  #12693 ) ;
#1621 = AXIS2_PLACEMENT_3D ( 'NONE', #10436, #14020, #5901 ) ;
#1622 = CARTESIAN_POINT ( 'NONE',  ( 21.98164641901421135, 11.39999970914575833, -0.3335879563140091153 ) ) ;
#1623 = EDGE_CURVE ( 'NONE', #4755, #14843, #9568, .T. ) ;
#1624 = DIRECTION ( 'NONE',  ( 0.000000000000000000, 0.000000000000000000, 1.000000000000000000 ) ) ;
#1625 = ORIENTED_EDGE ( 'NONE', *, *, #9039, .T. ) ;
#1626 = DIRECTION ( 'NONE',  ( -1.000000000000000000, 0.000000000000000000, 0.000000000000000000 ) ) ;
#1627 = ORIENTED_EDGE ( 'NONE', *, *, #8184, .F. ) ;
#1628 = VERTEX_POINT ( 'NONE', #500 ) ;
#1629 = ORIENTED_EDGE ( 'NONE', *, *, #1265, .T. ) ;
#1630 = AXIS2_PLACEMENT_3D ( 'NONE', #8697, #5453, #7701 ) ;
#1631 = ORIENTED_EDGE ( 'NONE', *, *, #13248, .F. ) ;
#1632 = EDGE_LOOP ( 'NONE', ( #12709, #14728 ) ) ;
#1633 = TOROIDAL_SURFACE ( 'NONE', #7823, 3.299999999999474909, 0.2000000000005234813 ) ;
#1634 = DIRECTION ( 'NONE',  ( 0.000000000000000000, 0.000000000000000000, -1.000000000000000000 ) ) ;
#1635 = AXIS2_PLACEMENT_3D ( 'NONE', #11045, #4929, #12135 ) ;
#1636 = CARTESIAN_POINT ( 'NONE',  ( 0.7342756466162075890, -1.803750000000060361, -3.698544502508174681 ) ) ;
#1637 = FACE_OUTER_BOUND ( 'NONE', #5202, .T. ) ;
#1638 = CARTESIAN_POINT ( 'NONE',  ( 1.127871658241229147, -3.796875000000003553, 3.713209756639876069 ) ) ;
#1639 = DIRECTION ( 'NONE',  ( -0.000000000000000000, -0.000000000000000000, -1.000000000000000000 ) ) ;
#1640 = EDGE_CURVE ( 'NONE', #1459, #11930, #5235, .T. ) ;
#1641 = CARTESIAN_POINT ( 'NONE',  ( -80.52077156573417938, 110.1741184958670061, -152.4984795835769944 ) ) ;
#1642 = DIRECTION ( 'NONE',  ( 0.000000000000000000, 0.000000000000000000, -1.000000000000000000 ) ) ;
#1643 = CARTESIAN_POINT ( 'NONE',  ( -77.82438362644001018, 82.17411849586700612, -80.14847958357698587 ) ) ;
#1644 = CARTESIAN_POINT ( 'NONE',  ( -4.435020996998821019, 11.99999970914572778, 69.03723529703218276 ) ) ;
#1645 = DIRECTION ( 'NONE',  ( 0.000000000000000000, 1.000000000000000000, 0.000000000000000000 ) ) ;
#1646 = EDGE_CURVE ( 'NONE', #13582, #558, #4646, .T. ) ;
#1647 = CARTESIAN_POINT ( 'NONE',  ( 16.75000000000000000, -0.2038245569916320166, -21.77831216351300014 ) ) ;
#1648 = VECTOR ( 'NONE', #1960, 1000.000000000000000 ) ;
#1649 = ORIENTED_EDGE ( 'NONE', *, *, #9028, .T. ) ;
#1650 = VECTOR ( 'NONE', #4516, 1000.000000000000114 ) ;
#1651 = CARTESIAN_POINT ( 'NONE',  ( -12.81835358098578403, 11.99999970914575798, -0.3335879563140091153 ) ) ;
#1652 = EDGE_LOOP ( 'NONE', ( #11220, #6715, #9351, #2408 ) ) ;
#1653 = ORIENTED_EDGE ( 'NONE', *, *, #12485, .F. ) ;
#1654 = ORIENTED_EDGE ( 'NONE', *, *, #9802, .T. ) ;
#1655 = CARTESIAN_POINT ( 'NONE',  ( 2.085982869228584224, -5.444374999999953779, 2.543086608318696928 ) ) ;
#1656 = EDGE_CURVE ( 'NONE', #3101, #11082, #1671, .T. ) ;
#1657 = DIRECTION ( 'NONE',  ( 0.000000000000000000, 0.000000000000000000, 1.000000000000000000 ) ) ;
#1658 = AXIS2_PLACEMENT_3D ( 'NONE', #14905, #12446, #6648 ) ;
#1659 = CARTESIAN_POINT ( 'NONE',  ( 1.242853247313944420, -5.772499999999809006, -2.998378529913433344 ) ) ;
#1660 = DIRECTION ( 'NONE',  ( 0.000000000000000000, 0.000000000000000000, -1.000000000000000000 ) ) ;
#1661 = DIRECTION ( 'NONE',  ( 0.000000000000000000, -1.000000000000000000, 0.000000000000000000 ) ) ;
#1662 = EDGE_CURVE ( 'NONE', #15166, #12591, #13571, .T. ) ;
#1663 = LINE ( 'NONE', #562, #8572 ) ;
#1664 = LINE ( 'NONE', #8793, #9089 ) ;
#1665 = CARTESIAN_POINT ( 'NONE',  ( -69.77438362644100778, 82.17411849586699191, -79.49847958357700861 ) ) ;
#1666 = EDGE_CURVE ( 'NONE', #506, #877, #569, .T. ) ;
#1667 = CARTESIAN_POINT ( 'NONE',  ( -77.52077156573416516, 59.67411849586701322, -152.4984795835769944 ) ) ;
#1668 = EDGE_CURVE ( 'NONE', #15237, #1406, #14768, .T. ) ;
#1669 = ORIENTED_EDGE ( 'NONE', *, *, #15306, .T. ) ;
#1670 = VECTOR ( 'NONE', #10957, 1000.000000000000000 ) ;
#1671 = LINE ( 'NONE', #11358, #13323 ) ;
#1672 = VECTOR ( 'NONE', #12373, 1000.000000000000000 ) ;
#1673 = ORIENTED_EDGE ( 'NONE', *, *, #13413, .T. ) ;
#1674 = FILL_AREA_STYLE_COLOUR ( '', #2124 ) ;
#1675 = ADVANCED_FACE ( 'NONE', ( #724, #8877 ), #7720, .T. ) ;
#1676 = CARTESIAN_POINT ( 'NONE',  ( 3.820852842225918700, -2.953124999999806821, 1.157524667501716786 ) ) ;
#1677 = ORIENTED_EDGE ( 'NONE', *, *, #12378, .F. ) ;
#1678 = CARTESIAN_POINT ( 'NONE',  ( 15.50000000000000000, -1.037157890325000054, -18.50000000000000000 ) ) ;
#1679 = ADVANCED_FACE ( 'NONE', ( #12747 ), #9399, .F. ) ;
#1680 = LINE ( 'NONE', #3854, #7097 ) ;
#1681 = AXIS2_PLACEMENT_3D ( 'NONE', #2035, #8163, #9320 ) ;
#1682 = CARTESIAN_POINT ( 'NONE',  ( -69.77438362644001302, 90.17411849586700612, -79.49847958357700861 ) ) ;
#1683 = DIRECTION ( 'NONE',  ( 0.000000000000000000, 0.000000000000000000, 1.000000000000000000 ) ) ;
#1684 = CARTESIAN_POINT ( 'NONE',  ( 16.75000000000000000, -0.2038245569916320166, 23.22168783648699986 ) ) ;
#1685 = DIRECTION ( 'NONE',  ( -0.000000000000000000, 1.000000000000000000, 0.000000000000000000 ) ) ;
#1686 = DIRECTION ( 'NONE',  ( 0.9961946980917453232, 0.000000000000000000, 0.08715574274766210716 ) ) ;
#1687 = ORIENTED_EDGE ( 'NONE', *, *, #14425, .F. ) ;
#1688 = VERTEX_POINT ( 'NONE', #3279 ) ;
#1689 = VECTOR ( 'NONE', #7984, 1000.000000000000000 ) ;
#1690 = DIRECTION ( 'NONE',  ( 0.9999934663667179313, -1.567696289299852414E-18, 0.003614861529252313445 ) ) ;
#1691 = CARTESIAN_POINT ( 'NONE',  ( 0.7459506331255062461, -1.366249999999944897, 3.755271276440845796 ) ) ;
#1692 = ORIENTED_EDGE ( 'NONE', *, *, #11601, .T. ) ;
#1693 = LINE ( 'NONE', #14485, #8282 ) ;
#1694 = CARTESIAN_POINT ( 'NONE',  ( -16.75000000000000000, -2.500000000000000000, 23.22168783648699986 ) ) ;
#1695 = LINE ( 'NONE', #528, #14945 ) ;
#1696 = CIRCLE ( 'NONE', #4685, 4.500000000000000888 ) ;
#1697 = LINE ( 'NONE', #14570, #8886 ) ;
#1698 = DIRECTION ( 'NONE',  ( 0.9375000000000004441, 0.000000000000000000, 0.3479852726768752902 ) ) ;
#1699 = CARTESIAN_POINT ( 'NONE',  ( 16.75000000000000000, -2.500000000000000000, -23.22168783648699986 ) ) ;
#1700 = ORIENTED_EDGE ( 'NONE', *, *, #2607, .T. ) ;
#1701 = CARTESIAN_POINT ( 'NONE',  ( -101.2743836264399988, 57.67411849586700612, -79.49847958357700861 ) ) ;
#1702 = ORIENTED_EDGE ( 'NONE', *, *, #11480, .T. ) ;
#1703 = ORIENTED_EDGE ( 'NONE', *, *, #6023, .F. ) ;
#1704 = ORIENTED_EDGE ( 'NONE', *, *, #2972, .F. ) ;
#1705 = ORIENTED_EDGE ( 'NONE', *, *, #14847, .F. ) ;
#1706 = VERTEX_POINT ( 'NONE', #14214 ) ;
#1707 = LINE ( 'NONE', #11168, #13498 ) ;
#1708 = CARTESIAN_POINT ( 'NONE',  ( 3.783562653031121936, -1.569374999999871845, 0.3712484392075319217 ) ) ;
#1709 = EDGE_CURVE ( 'NONE', #8759, #14946, #15292, .T. ) ;
#1710 = CARTESIAN_POINT ( 'NONE',  ( -65.78565528768382364, 67.29799558322736175, -83.44847958357698303 ) ) ;
#1711 = CARTESIAN_POINT ( 'NONE',  ( -1.491583768208377681, -3.687499999999984901, 3.598334897712680114 ) ) ;
#1712 = CARTESIAN_POINT ( 'NONE',  ( 14.25000000000000178, -0.2714405302574905421, -22.01253933645463690 ) ) ;
#1713 = CARTESIAN_POINT ( 'NONE',  ( 15.70366306705349757, -0.2717122460102775472, 21.17420925361331641 ) ) ;
#1714 = DIRECTION ( 'NONE',  ( -1.000000000000000000, 0.000000000000000000, 0.000000000000000000 ) ) ;
#1715 = CARTESIAN_POINT ( 'NONE',  ( -15.50000000000000000, -5.000000000000000000, 18.50000000000000000 ) ) ;
#1716 = CARTESIAN_POINT ( 'NONE',  ( 57.41329019055577021, 2.488961461112888074, 129.5095611191910621 ) ) ;
#1717 = DIRECTION ( 'NONE',  ( 0.000000000000000000, 0.000000000000000000, 1.000000000000000000 ) ) ;
#1718 = LINE ( 'NONE', #405, #1584 ) ;
#1719 = ORIENTED_EDGE ( 'NONE', *, *, #2228, .T. ) ;
#1720 = DIRECTION ( 'NONE',  ( 0.000000000000000000, 0.000000000000000000, -1.000000000000000000 ) ) ;
#1721 = EDGE_LOOP ( 'NONE', ( #15325, #9614, #7601, #1653, #1702 ) ) ;
#1722 = ORIENTED_EDGE ( 'NONE', *, *, #4298, .T. ) ;
#1723 = ORIENTED_EDGE ( 'NONE', *, *, #11348, .T. ) ;
#1724 = UNCERTAINTY_MEASURE_WITH_UNIT (LENGTH_MEASURE( 1.000000000000000082E-05 ), #10709, 'distance_accuracy_value', 'NONE');
#1725 = CARTESIAN_POINT ( 'NONE',  ( 1.260313249030111438, -5.397499999999716636, 3.044840626206112955 ) ) ;
#1726 = EDGE_CURVE ( 'NONE', #10851, #13125, #2192, .T. ) ;
#1727 = CARTESIAN_POINT ( 'NONE',  ( -69.77438362644001302, 90.17411849586700612, -58.99847958357700151 ) ) ;
#1728 = DIRECTION ( 'NONE',  ( 1.000000000000000000, 0.000000000000000000, 0.000000000000000000 ) ) ;
#1729 = DIRECTION ( 'NONE',  ( 0.000000000000000000, 0.000000000000000000, 1.000000000000000000 ) ) ;
#1730 = DIRECTION ( 'NONE',  ( 0.000000000000000000, 0.000000000000000000, 1.000000000000000000 ) ) ;
#1731 = LINE ( 'NONE', #14763, #1436 ) ;
#1732 = CARTESIAN_POINT ( 'NONE',  ( -4.296274425956841725, -0.5002988223950231017, 0.02453012155904704325 ) ) ;
#1733 = CARTESIAN_POINT ( 'NONE',  ( -1.864549691619314498, -4.928749999999819664, -2.792029179168366237 ) ) ;
#1734 = ORIENTED_EDGE ( 'NONE', *, *, #13246, .T. ) ;
#1735 = CARTESIAN_POINT ( 'NONE',  ( -69.77438362644100778, 82.17411849586699191, -67.49847958357700861 ) ) ;
#1736 = B_SPLINE_CURVE_WITH_KNOTS ( 'NONE', 3,
 ( #165, #3811, #1245, #4912, #10632, #13286, #11730, #8236, #10713, #1098, #6171, #10557, #2339, #8392, #12977, #7089, #11880, #13205, #2564, #7314, #13590, #7396, #8690, #10945, #4122, #1783, #12419, #2721, #7627, #6390, #13513, #11252, #11024, #8771, #13436, #11171, #1557, #7696, #8848, #2649, #2956, #3963, #6461, #5291, #2880, #306, #6537, #5055, #2798, #12348, #14736, #8920, #12267, #14809, #9770, #7549, #617, #1638, #5373, #10077, #476, #11103, #1711, #5211, #10002, #12186, #9924, #6312, #9852, #7468, #14657, #14505, #4196, #12118, #3891, #4042, #396, #1486, #545, #6238, #8617, #13364, #5142, #14583, #6913, #13736, #7844, #15034, #1863, #3327, #8060, #3182, #4349, #13658, #7910, #2163, #11633, #10144, #3108, #12578, #2086, #15104, #10452, #10223, #15183, #1940, #5520, #6757, #9073, #13879, #10379, #4570, #12641, #3028, #11328, #13813, #995, #2007, #5750, #13954, #11478, #14955, #7980, #844, #923, #6687, #5602, #11397, #10307, #762, #4423, #6620, #5684, #7771, #14876, #9142, #3248, #12502, #6838, #695, #11559, #4493, #5446, #9214, #4265, #12797, #13595, #5450, #7633, #9077, #13819, #8925, #10082, #4048, #13662, #7914, #2011, #550, #8852, #4126, #7849, #5526, #850, #623, #5606, #2961, #11259, #12508, #6465, #12646, #1788, #3033, #7775, #8997, #10149, #1868, #13742, #3112, #4201, #6763, #11483, #10311, #6626, #7700, #12423, #13518, #11175, #6541, #2884, #11333, #14813, #10227, #6692, #700, #11400, #14740, #14880, #5296, #8777, #5377 ),
 .UNSPECIFIED., .F., .F.,
 ( 4, 2, 2, 2, 2, 2, 2, 2, 2, 2, 2, 2, 2, 2, 2, 2, 2, 2, 2, 2, 2, 2, 2, 2, 2, 2, 2, 2, 2, 2, 2, 2, 2, 2, 2, 2, 2, 2, 2, 2, 2, 2, 2, 2, 2, 2, 2, 2, 2, 2, 2, 2, 2, 2, 2, 2, 2, 2, 2, 2, 2, 2, 2, 2, 2, 2, 2, 2, 2, 2, 2, 2, 2, 2, 2, 2, 2, 2, 2, 2, 2, 2, 2, 2, 2, 2, 2, 2, 2, 2, 2, 2, 2, 2, 2, 2, 2, 2, 2, 4 ),
 ( 0.06608205603566359720, 0.07031250000000000000, 0.07812500000000000000, 0.08593750000000000000, 0.09375000000000000000, 0.1015625000000000000, 0.1093750000000000000, 0.1171875000000000000, 0.1250000000000000000, 0.1328125000000000000, 0.1406250000000000000, 0.1484375000000000000, 0.1562500000000000000, 0.1640625000000000000, 0.1718750000000000000, 0.1796875000000000000, 0.1875000000000000000, 0.1953125000000000000, 0.2031250000000000000, 0.2109375000000000000, 0.2187500000000000000, 0.2265625000000000000, 0.2343750000000000000, 0.2421875000000000000, 0.2500000000000000000, 0.2578125000000000555, 0.2656250000000000000, 0.2734375000000000000, 0.2812500000000000000, 0.2890625000000000000, 0.2968750000000000000, 0.3046875000000000000, 0.3125000000000000000, 0.3203125000000000000, 0.3281250000000000000, 0.3359375000000000000, 0.3437500000000000000, 0.3515625000000000000, 0.3593750000000000000, 0.3671875000000000000, 0.3750000000000000000, 0.3828125000000000000, 0.3906250000000000000, 0.3984375000000000000, 0.4062499999999999445, 0.4140625000000000000, 0.4218750000000000000, 0.4296875000000000000, 0.4375000000000000000, 0.4453125000000000000, 0.4531250000000000000, 0.4609375000000000555, 0.4687500000000000000, 0.4765624999999999445, 0.4843750000000000000, 0.4921875000000000000, 0.5000000000000000000, 0.5078125000000000000, 0.5156250000000000000, 0.5234375000000000000, 0.5312500000000000000, 0.5390625000000000000, 0.5468750000000001110, 0.5546875000000000000, 0.5625000000000000000, 0.5703125000000000000, 0.5781250000000000000, 0.5859375000000000000, 0.5937500000000000000, 0.6015625000000000000, 0.6093750000000000000, 0.6171875000000000000, 0.6250000000000000000, 0.6328125000000000000, 0.6406250000000000000, 0.6484375000000000000, 0.6562500000000000000, 0.6640625000000000000, 0.6718750000000000000, 0.6796875000000000000, 0.6875000000000000000, 0.6953125000000000000, 0.7031250000000000000, 0.7109375000000000000, 0.7187500000000000000, 0.7265625000000000000, 0.7343750000000000000, 0.7421875000000001110, 0.7500000000000000000, 0.7578125000000000000, 0.7656250000000000000, 0.7734374999999998890, 0.7812500000000000000, 0.7890625000000000000, 0.7968750000000000000, 0.8046875000000000000, 0.8125000000000000000, 0.8203125000000000000, 0.8281250000000001110, 0.8331820081006554579 ),
 .UNSPECIFIED. ) ;
#1737 = ADVANCED_FACE ( 'NONE', ( #12669 ), #8168, .F. ) ;
#1738 = ORIENTED_EDGE ( 'NONE', *, *, #2710, .T. ) ;
#1739 = PRODUCT ( 'Sliding Jaws', 'Sliding Jaws', '', ( #3689 ) ) ;
#1740 = CARTESIAN_POINT ( 'NONE',  ( -1.169542390366794304, -2.703125000000013323, 3.851808151836873861 ) ) ;
#1741 = ORIENTED_EDGE ( 'NONE', *, *, #10652, .T. ) ;
#1742 = ADVANCED_FACE ( 'NONE', ( #1185 ), #872, .F. ) ;
#1743 = DIRECTION ( 'NONE',  ( -1.000000000000000000, 0.000000000000000000, 0.000000000000000000 ) ) ;
#1744 = DIRECTION ( 'NONE',  ( 0.9961946980917452121, -3.779777825264104572E-17, 0.08715574274766174634 ) ) ;
#1745 = CARTESIAN_POINT ( 'NONE',  ( -5.196152422706634688, 1.678847577293359539, -8.911270275552416508E-16 ) ) ;
#1746 = EDGE_CURVE ( 'NONE', #12096, #14091, #2664, .T. ) ;
#1747 = CARTESIAN_POINT ( 'NONE',  ( -1.006616814747114065E-29, -2.568816543514387226E-44, 0.000000000000000000 ) ) ;
#1748 = CARTESIAN_POINT ( 'NONE',  ( -52.77438362643999881, 65.17411849586700612, -145.4984795835769944 ) ) ;
#1749 = ADVANCED_FACE ( 'NONE', ( #8009 ), #2911, .F. ) ;
#1750 = DIRECTION ( 'NONE',  ( 1.000000000000000000, -0.000000000000000000, 0.000000000000000000 ) ) ;
#1751 = CARTESIAN_POINT ( 'NONE',  ( -69.77438362644001302, 110.1741184958670061, -152.4984795835769944 ) ) ;
#1752 = CARTESIAN_POINT ( 'NONE',  ( -12.81835358098578403, 11.99999970914575975, -8.183940086454237317 ) ) ;
#1753 = VERTEX_POINT ( 'NONE', #14134 ) ;
#1754 =( NAMED_UNIT ( * ) SI_UNIT ( $, .STERADIAN. ) SOLID_ANGLE_UNIT ( ) );
#1755 = EDGE_CURVE ( 'NONE', #8497, #5254, #8091, .T. ) ;
#1756 = EDGE_LOOP ( 'NONE', ( #4563, #10317, #4029, #4206, #11393, #10915 ) ) ;
#1757 = AXIS2_PLACEMENT_3D ( 'NONE', #13264, #3946, #2774 ) ;
#1758 = CARTESIAN_POINT ( 'NONE',  ( -54.81638362644000040, 63.99516924618178848, -147.9984795835769944 ) ) ;
#1759 = CARTESIAN_POINT ( 'NONE',  ( 3.518605591592443016, -1.522500000000036380, 1.455944046807712500 ) ) ;
#1760 = EDGE_LOOP ( 'NONE', ( #9418, #4584, #11504, #11247, #110, #7784 ) ) ;
#1761 = ADVANCED_FACE ( 'NONE', ( #10643, #2117 ), #8245, .F. ) ;
#1762 = EDGE_CURVE ( 'NONE', #4888, #4114, #15061, .T. ) ;
#1763 = CARTESIAN_POINT ( 'NONE',  ( 0.000000000000000000, 0.000000000000000000, 0.000000000000000000 ) ) ;
#1764 = CIRCLE ( 'NONE', #3492, 0.6000000000000000888 ) ;
#1765 = CARTESIAN_POINT ( 'NONE',  ( -1.764029795486899532, -5.202224379335410376, -3.099337613330489738 ) ) ;
#1766 = FACE_OUTER_BOUND ( 'NONE', #14367, .T. ) ;
#1767 = CARTESIAN_POINT ( 'NONE',  ( -9.503456061879925088, 11.99999970914574021, 69.60114695342350899 ) ) ;
#1768 = DIRECTION ( 'NONE',  ( -0.000000000000000000, 1.000000000000000000, 4.336808689942017736E-16 ) ) ;
#1769 = DIRECTION ( 'NONE',  ( 0.000000000000000000, 0.000000000000000000, 1.000000000000000000 ) ) ;
#1770 = ORIENTED_EDGE ( 'NONE', *, *, #2864, .T. ) ;
#1771 = CARTESIAN_POINT ( 'NONE',  ( -15.50000000000000000, -0.2038245569916614930, 23.94337567297399971 ) ) ;
#1772 = ORIENTED_EDGE ( 'NONE', *, *, #13010, .F. ) ;
#1773 = VECTOR ( 'NONE', #14677, 1000.000000000000000 ) ;
#1774 = VERTEX_POINT ( 'NONE', #4756 ) ;
#1775 = ORIENTED_EDGE ( 'NONE', *, *, #888, .F. ) ;
#1776 = ORIENTED_EDGE ( 'NONE', *, *, #6424, .F. ) ;
#1777 = ORIENTED_EDGE ( 'NONE', *, *, #12434, .T. ) ;
#1778 = AXIS2_PLACEMENT_3D ( 'NONE', #10159, #14891, #7310 ) ;
#1779 = CARTESIAN_POINT ( 'NONE',  ( -15.50000000000000000, -1.037157890325000054, 26.00000000000000000 ) ) ;
#1780 = CIRCLE ( 'NONE', #9948, 1.250000000000001110 ) ;
#1781 = CARTESIAN_POINT ( 'NONE',  ( -3.115386749435359093, -1.991250000000079678, -2.079980318098562098 ) ) ;
#1782 = DIRECTION ( 'NONE',  ( 0.000000000000000000, 0.000000000000000000, 1.000000000000000000 ) ) ;
#1783 = CARTESIAN_POINT ( 'NONE',  ( -3.618276846414829162, -4.546874999999968914, 1.099041561241040466 ) ) ;
#1784 = LINE ( 'NONE', #4043, #7266 ) ;
#1785 = LINE ( 'NONE', #9447, #8840 ) ;
#1786 = CIRCLE ( 'NONE', #8475, 2.500000000000002220 ) ;
#1787 = DIRECTION ( 'NONE',  ( -0.000000000000000000, -0.000000000000000000, 1.000000000000000000 ) ) ;
#1788 = CARTESIAN_POINT ( 'NONE',  ( 2.351042318464003689, -1.156249999999995559, -3.516557504029556913 ) ) ;
#1789 = CARTESIAN_POINT ( 'NONE',  ( -88.81638362644100937, 97.99516924618178848, -147.9984795835769944 ) ) ;
#1790 = DIRECTION ( 'NONE',  ( 0.000000000000000000, -1.000000000000000000, 0.000000000000000000 ) ) ;
#1791 = DIRECTION ( 'NONE',  ( 9.422394424380274864E-16, -1.000000000000000000, 0.000000000000000000 ) ) ;
#1792 = VERTEX_POINT ( 'NONE', #11655 ) ;
#1793 = DIRECTION ( 'NONE',  ( 0.4226182617407006625, -0.9063077870366492705, 0.000000000000000000 ) ) ;
#1794 = CIRCLE ( 'NONE', #10202, 16.06499999999999773 ) ;
#1795 = VERTEX_POINT ( 'NONE', #12899 ) ;
#1796 = ORIENTED_EDGE ( 'NONE', *, *, #490, .F. ) ;
#1797 = ORIENTED_EDGE ( 'NONE', *, *, #2706, .F. ) ;
#1798 = DIRECTION ( 'NONE',  ( 1.000000000000000000, 0.000000000000000000, 0.000000000000000000 ) ) ;
#1799 = CARTESIAN_POINT ( 'NONE',  ( -0.6299995022919476773, -5.866249999999999964, -3.171388681290751244 ) ) ;
#1800 = FACE_OUTER_BOUND ( 'NONE', #11038, .T. ) ;
#1801 = CIRCLE ( 'NONE', #10466, 1.250000000000001110 ) ;
#1802 = CARTESIAN_POINT ( 'NONE',  ( -3.897114317029972685, -9.945166405816852549E-15, -2.249999999999999112 ) ) ;
#1803 = LINE ( 'NONE', #5314, #5906 ) ;
#1804 = DIRECTION ( 'NONE',  ( 0.000000000000000000, 0.000000000000000000, 1.000000000000000000 ) ) ;
#1805 = ADVANCED_FACE ( 'NONE', ( #6936 ), #11505, .T. ) ;
#1806 = AXIS2_PLACEMENT_3D ( 'NONE', #6432, #13562, #2759 ) ;
#1807 = CARTESIAN_POINT ( 'NONE',  ( 0.9968050443165101804, -4.381875000000003517, 3.281628308787421400 ) ) ;
#1808 = ORIENTED_EDGE ( 'NONE', *, *, #243, .T. ) ;
#1809 = DIRECTION ( 'NONE',  ( -0.000000000000000000, -0.000000000000000000, 1.000000000000000000 ) ) ;
#1810 = EDGE_CURVE ( 'NONE', #2099, #14169, #6864, .T. ) ;
#1811 = EDGE_LOOP ( 'NONE', ( #11659, #8970, #5653 ) ) ;
#1812 = CIRCLE ( 'NONE', #8000, 4.000000000000000000 ) ;
#1813 = VERTEX_POINT ( 'NONE', #6788 ) ;
#1814 = CIRCLE ( 'NONE', #9238, 0.2500000000000000000 ) ;
#1815 = CARTESIAN_POINT ( 'NONE',  ( 3.986138996993924266, -2.999999999999990674, -0.001451045610905104914 ) ) ;
#1816 = ORIENTED_EDGE ( 'NONE', *, *, #1656, .F. ) ;
#1817 = VECTOR ( 'NONE', #4025, 1000.000000000000000 ) ;
#1818 = FACE_OUTER_BOUND ( 'NONE', #14215, .T. ) ;
#1819 = DIRECTION ( 'NONE',  ( 1.000000000000000000, 0.000000000000000000, 0.000000000000000000 ) ) ;
#1820 = CARTESIAN_POINT ( 'NONE',  ( -57.27438362644000591, 99.17411849586700612, -145.4984795835769660 ) ) ;
#1821 = EDGE_CURVE ( 'NONE', #6249, #3634, #5632, .T. ) ;
#1822 = AXIS2_PLACEMENT_3D ( 'NONE', #9717, #12067, #7575 ) ;
#1823 = EDGE_CURVE ( 'NONE', #8050, #4503, #5863, .T. ) ;
#1824 = CIRCLE ( 'NONE', #10491, 0.5999999999999999778 ) ;
#1825 = DIRECTION ( 'NONE',  ( 0.000000000000000000, -1.000000000000000000, -0.000000000000000000 ) ) ;
#1826 = CARTESIAN_POINT ( 'NONE',  ( 1.771711357477687043, 2.042612654300325570, 4.500000000000000000 ) ) ;
#1827 = DIRECTION ( 'NONE',  ( 0.000000000000000000, 0.000000000000000000, -1.000000000000000000 ) ) ;
#1828 = CARTESIAN_POINT ( 'NONE',  ( -69.77438362644001302, 82.17411849586700612, -79.59847958357700293 ) ) ;
#1829 = LINE ( 'NONE', #4240, #2275 ) ;
#1830 =( BOUNDED_CURVE ( )  B_SPLINE_CURVE ( 3, ( #7733, #5488, #13923, #9035 ),
 .UNSPECIFIED., .F., .T. ) 
 B_SPLINE_CURVE_WITH_KNOTS ( ( 4, 4 ),
 ( -2.664535259100375697E-15, 1.570796326794896780 ),
 .UNSPECIFIED. ) 
 CURVE ( )  GEOMETRIC_REPRESENTATION_ITEM ( )  RATIONAL_B_SPLINE_CURVE ( ( 1.000000000000000000, 0.8047378541243643824, 0.8047378541243643824, 1.000000000000000000 ) ) 
 REPRESENTATION_ITEM ( '' )  );
#1831 = DIRECTION ( 'NONE',  ( 0.000000000000000000, 0.000000000000000000, 1.000000000000000000 ) ) ;
#1832 = ORIENTED_EDGE ( 'NONE', *, *, #9595, .T. ) ;
#1833 = CARTESIAN_POINT ( 'NONE',  ( 17.12895037488186389, -11.13829663063783215, 0.2687305842673423095 ) ) ;
#1834 = CARTESIAN_POINT ( 'NONE',  ( 1.096135970525343728, -1.788124999999989750, -3.610092524386872004 ) ) ;
#1835 = ORIENTED_EDGE ( 'NONE', *, *, #143, .T. ) ;
#1836 = AXIS2_PLACEMENT_3D ( 'NONE', #14259, #1069, #12023 ) ;
#1837 = AXIS2_PLACEMENT_3D ( 'NONE', #11615, #4553, #10513 ) ;
#1838 = EDGE_CURVE ( 'NONE', #3798, #13165, #8107, .T. ) ;
#1839 = CARTESIAN_POINT ( 'NONE',  ( -88.81638362644000040, 66.35306774555222376, -150.4984795835770228 ) ) ;
#1840 = ADVANCED_FACE ( 'NONE', ( #8330 ), #3823, .T. ) ;
#1841 = DIRECTION ( 'NONE',  ( -1.287488025362404182E-15, -1.000000000000000000, 0.000000000000000000 ) ) ;
#1842 = DIRECTION ( 'NONE',  ( 0.000000000000000000, 0.000000000000000000, 1.000000000000000000 ) ) ;
#1843 = CYLINDRICAL_SURFACE ( 'NONE', #13932, 4.000000000000000000 ) ;
#1844 = CARTESIAN_POINT ( 'NONE',  ( -14.25000000000000000, -0.2038245569916330158, -21.77831216351300014 ) ) ;
#1845 = AXIS2_PLACEMENT_3D ( 'NONE', #6288, #2386, #4884 ) ;
#1846 = AXIS2_PLACEMENT_3D ( 'NONE', #12744, #2113, #3999 ) ;
#1847 = EDGE_CURVE ( 'NONE', #4668, #14787, #1127, .T. ) ;
#1848 = DIRECTION ( 'NONE',  ( 1.000000000000000000, 0.000000000000000000, 0.000000000000000000 ) ) ;
#1849 = ADVANCED_FACE ( 'NONE', ( #3740 ), #1334, .F. ) ;
#1850 = EDGE_LOOP ( 'NONE', ( #8013, #13009, #13275, #13946 ) ) ;
#1851 = CARTESIAN_POINT ( 'NONE',  ( -88.81638362644100937, 100.3530677455522238, -150.4984795835770228 ) ) ;
#1852 = ORIENTED_EDGE ( 'NONE', *, *, #5042, .F. ) ;
#1853 = ORIENTED_EDGE ( 'NONE', *, *, #1810, .F. ) ;
#1854 = ORIENTED_EDGE ( 'NONE', *, *, #5396, .F. ) ;
#1855 = VERTEX_POINT ( 'NONE', #8626 ) ;
#1856 = VERTEX_POINT ( 'NONE', #13298 ) ;
#1857 = CARTESIAN_POINT ( 'NONE',  ( -3.656031798353854168, -5.499213562373083342, 0.001347523837372742971 ) ) ;
#1858 = EDGE_CURVE ( 'NONE', #11015, #9386, #12079, .T. ) ;
#1859 = CARTESIAN_POINT ( 'NONE',  ( -3.224082633657694430, -0.9912500000000042943, -2.155484159616896989 ) ) ;
#1860 = VECTOR ( 'NONE', #5540, 1000.000000000000000 ) ;
#1861 = DIRECTION ( 'NONE',  ( 0.000000000000000000, -0.000000000000000000, 1.000000000000000000 ) ) ;
#1862 = CIRCLE ( 'NONE', #1614, 1.999999999999988010 ) ;
#1863 = CARTESIAN_POINT ( 'NONE',  ( 3.506874188274308413, -3.078124999999926281, -1.873277435140577429 ) ) ;
#1864 = LINE ( 'NONE', #13738, #14193 ) ;
#1865 = EDGE_CURVE ( 'NONE', #12872, #13910, #10889, .T. ) ;
#1866 = PLANE ( 'NONE',  #13318 ) ;
#1867 = DIRECTION ( 'NONE',  ( -1.000000000000000000, 0.000000000000000000, 0.000000000000000000 ) ) ;
#1868 = CARTESIAN_POINT ( 'NONE',  ( 4.164680137118252468, -1.031249999999941602, -0.8299691317567963189 ) ) ;
#1869 = DIRECTION ( 'NONE',  ( 0.000000000000000000, 0.000000000000000000, -1.000000000000000000 ) ) ;
#1870 = CARTESIAN_POINT ( 'NONE',  ( -104.2743836264399988, 101.6741184958670061, -79.49847958357700861 ) ) ;
#1871 = CARTESIAN_POINT ( 'NONE',  ( 16.75000000000000355, -0.2715193793361441177, 22.98718409945082897 ) ) ;
#1872 = ORIENTED_EDGE ( 'NONE', *, *, #5140, .T. ) ;
#1873 = CARTESIAN_POINT ( 'NONE',  ( -15.50000000000000000, -2.500000000000000000, -23.94337567297399971 ) ) ;
#1874 = PRESENTATION_LAYER_ASSIGNMENT (  '', '', ( #14245 ) ) ;
#1875 = EDGE_LOOP ( 'NONE', ( #14483, #1005, #11338, #4138 ) ) ;
#1876 = VECTOR ( 'NONE', #9651, 1000.000000000000000 ) ;
#1877 = ORIENTED_EDGE ( 'NONE', *, *, #6236, .F. ) ;
#1878 = ORIENTED_EDGE ( 'NONE', *, *, #2138, .T. ) ;
#1879 = AXIS2_PLACEMENT_3D ( 'NONE', #1991, #14862, #4332 ) ;
#1880 = FACE_OUTER_BOUND ( 'NONE', #11161, .T. ) ;
#1881 = CARTESIAN_POINT ( 'NONE',  ( 3.135427973343609231, -5.538124999999991971, 0.9519854854111799991 ) ) ;
#1882 = PLANE ( 'NONE',  #893 ) ;
#1883 = DIRECTION ( 'NONE',  ( 0.000000000000000000, 0.000000000000000000, -1.000000000000000000 ) ) ;
#1884 = LINE ( 'NONE', #12741, #5887 ) ;
#1885 = B_SPLINE_CURVE_WITH_KNOTS ( 'NONE', 3,
 ( #12579, #10078, #12349, #14658, #1712, #618 ),
 .UNSPECIFIED., .F., .F.,
 ( 4, 2, 4 ),
 ( 1.820537833122031657, 2.555393473688635897, 3.290249114255240137 ),
 .UNSPECIFIED. ) ;
#1886 = AXIS2_PLACEMENT_3D ( 'NONE', #8104, #8023, #806 ) ;
#1887 = DIRECTION ( 'NONE',  ( -0.000000000000000000, -0.000000000000000000, 1.000000000000000000 ) ) ;
#1888 = CARTESIAN_POINT ( 'NONE',  ( 2.709010606882195304, -0.4995676945082524467, 2.903689985453846489 ) ) ;
#1889 = AXIS2_PLACEMENT_3D ( 'NONE', #8733, #7514, #3860 ) ;
#1890 = FACE_OUTER_BOUND ( 'NONE', #3846, .T. ) ;
#1891 = CARTESIAN_POINT ( 'NONE',  ( -42.77438362644000591, 104.6741184958670061, -15.85886927678779834 ) ) ;
#1892 = ORIENTED_EDGE ( 'NONE', *, *, #9615, .T. ) ;
#1893 = CYLINDRICAL_SURFACE ( 'NONE', #1658, 4.499999999999997335 ) ;
#1894 = ORIENTED_EDGE ( 'NONE', *, *, #8577, .T. ) ;
#1895 = DIRECTION ( 'NONE',  ( 0.000000000000000000, -1.000000000000000000, 0.000000000000000000 ) ) ;
#1896 = AXIS2_PLACEMENT_3D ( 'NONE', #9000, #1565, #11335 ) ;
#1897 = ORIENTED_EDGE ( 'NONE', *, *, #2710, .F. ) ;
#1898 = CIRCLE ( 'NONE', #12793, 4.500000000000003553 ) ;
#1899 = CARTESIAN_POINT ( 'NONE',  ( 3.689984836354881281, -2.937500000000126565, 1.529580092797385715 ) ) ;
#1900 = ORIENTED_EDGE ( 'NONE', *, *, #15000, .T. ) ;
#1901 = DIRECTION ( 'NONE',  ( 1.000000000000000000, 0.000000000000000000, 1.224646799147353207E-16 ) ) ;
#1902 = ADVANCED_FACE ( 'NONE', ( #3673 ), #911, .F. ) ;
#1903 = DIRECTION ( 'NONE',  ( 0.000000000000000000, 0.000000000000000000, 1.000000000000000000 ) ) ;
#1904 = CARTESIAN_POINT ( 'NONE',  ( 14.25000000000000000, -0.3156864504677177052, 22.25638000318208753 ) ) ;
#1905 = AXIS2_PLACEMENT_3D ( 'NONE', #12918, #14003, #6951 ) ;
#1906 = VECTOR ( 'NONE', #3184, 1000.000000000000000 ) ;
#1907 = FACE_OUTER_BOUND ( 'NONE', #205, .T. ) ;
#1908 = DIRECTION ( 'NONE',  ( -1.224646799147353207E-16, -2.139562256385042123E-31, 1.000000000000000000 ) ) ;
#1909 = DIRECTION ( 'NONE',  ( 0.8660254037844387076, 0.4999999999999998890, 0.000000000000000000 ) ) ;
#1910 = FACE_OUTER_BOUND ( 'NONE', #9957, .T. ) ;
#1911 = CARTESIAN_POINT ( 'NONE',  ( -86.77438362644001302, 99.17411849586700612, -86.49847958357699440 ) ) ;
#1912 = VERTEX_POINT ( 'NONE', #14593 ) ;
#1913 = DIRECTION ( 'NONE',  ( 0.000000000000000000, -1.000000000000000000, 0.000000000000000000 ) ) ;
#1914 = CARTESIAN_POINT ( 'NONE',  ( -3.657957510581538951, -2.116249999999859632, 0.7266254446581354998 ) ) ;
#1915 = VERTEX_POINT ( 'NONE', #13216 ) ;
#1916 = EDGE_CURVE ( 'NONE', #6810, #5926, #9087, .T. ) ;
#1917 = AXIS2_PLACEMENT_3D ( 'NONE', #7126, #12857, #11684 ) ;
#1918 = DIRECTION ( 'NONE',  ( -1.000000000000000000, 0.000000000000000000, 0.000000000000000000 ) ) ;
#1919 = EDGE_CURVE ( 'NONE', #13427, #12323, #4840, .T. ) ;
#1920 = CARTESIAN_POINT ( 'NONE',  ( -64.53565528768383786, 67.29799558322736175, -83.44847958357698303 ) ) ;
#1921 = FACE_OUTER_BOUND ( 'NONE', #3534, .T. ) ;
#1922 =( BOUNDED_CURVE ( )  B_SPLINE_CURVE ( 3, ( #2090, #6622, #1942, #6689 ),
 .UNSPECIFIED., .F., .T. ) 
 B_SPLINE_CURVE_WITH_KNOTS ( ( 4, 4 ),
 ( 1.570796326794896780, 3.141592653589795336 ),
 .UNSPECIFIED. ) 
 CURVE ( )  GEOMETRIC_REPRESENTATION_ITEM ( )  RATIONAL_B_SPLINE_CURVE ( ( 1.000000000000000000, 0.8047378541243644934, 0.8047378541243644934, 1.000000000000000000 ) ) 
 REPRESENTATION_ITEM ( '' )  );
#1923 = FACE_OUTER_BOUND ( 'NONE', #2301, .T. ) ;
#1924 = DIRECTION ( 'NONE',  ( 0.000000000000000000, 1.000000000000000000, 0.000000000000000000 ) ) ;
#1925 = CARTESIAN_POINT ( 'NONE',  ( -52.77438362644000591, 65.17411849586700612, -145.4984795835769660 ) ) ;
#1926 = CIRCLE ( 'NONE', #12335, 8.000000000000007105 ) ;
#1927 = VERTEX_POINT ( 'NONE', #4988 ) ;
#1928 = DIRECTION ( 'NONE',  ( 0.000000000000000000, 0.000000000000000000, 1.000000000000000000 ) ) ;
#1929 = ORIENTED_EDGE ( 'NONE', *, *, #7103, .F. ) ;
#1930 = ORIENTED_EDGE ( 'NONE', *, *, #1823, .F. ) ;
#1931 = EDGE_LOOP ( 'NONE', ( #1878, #2814, #12530, #10627 ) ) ;
#1932 = ORIENTED_EDGE ( 'NONE', *, *, #2223, .T. ) ;
#1933 = EDGE_CURVE ( 'NONE', #14725, #14787, #2400, .T. ) ;
#1934 = ORIENTED_EDGE ( 'NONE', *, *, #3377, .T. ) ;
#1935 = CARTESIAN_POINT ( 'NONE',  ( 2.975116562878357129, -6.092963562372954556, -1.986801736614415947 ) ) ;
#1936 = CARTESIAN_POINT ( 'NONE',  ( 2.195116763761142398, -0.4287499999998638511, 3.287093781494352385 ) ) ;
#1937 = EDGE_CURVE ( 'NONE', #12753, #10723, #4388, .T. ) ;
#1938 = VECTOR ( 'NONE', #4896, 1000.000000000000000 ) ;
#1939 = FILL_AREA_STYLE_COLOUR ( '', #12281 ) ;
#1940 = CARTESIAN_POINT ( 'NONE',  ( -1.898222722261231343, -2.671874999999975131, 3.554431989243950873 ) ) ;
#1941 = LINE ( 'NONE', #7628, #5786 ) ;
#1942 = CARTESIAN_POINT ( 'NONE',  ( 1.581646419014215876, 11.75147157172189871, 0.2664120436859918062 ) ) ;
#1943 = CARTESIAN_POINT ( 'NONE',  ( -47.27438362644100778, 114.1741184958670061, -67.49847958357700861 ) ) ;
#1944 = DIRECTION ( 'NONE',  ( -1.000000000000000000, -7.475397945009582610E-16, 0.000000000000000000 ) ) ;
#1945 = FACE_BOUND ( 'NONE', #3595, .T. ) ;
#1946 = CARTESIAN_POINT ( 'NONE',  ( 17.18164641901421419, 3.654316742536407592, 0.2664120436859910845 ) ) ;
#1947 = DIRECTION ( 'NONE',  ( -0.000000000000000000, -0.000000000000000000, 1.000000000000000000 ) ) ;
#1948 = EDGE_CURVE ( 'NONE', #15131, #14575, #12129, .T. ) ;
#1949 = ORIENTED_EDGE ( 'NONE', *, *, #7451, .F. ) ;
#1950 = ORIENTED_EDGE ( 'NONE', *, *, #6979, .T. ) ;
#1951 = VECTOR ( 'NONE', #15321, 1000.000000000000114 ) ;
#1952 = VERTEX_POINT ( 'NONE', #5151 ) ;
#1953 = ORIENTED_EDGE ( 'NONE', *, *, #53, .T. ) ;
#1954 = EDGE_CURVE ( 'NONE', #11451, #10071, #9980, .T. ) ;
#1955 = CYLINDRICAL_SURFACE ( 'NONE', #9456, 16.00000000000000000 ) ;
#1956 = ADVANCED_FACE ( 'NONE', ( #2427 ), #1255, .F. ) ;
#1957 = ADVANCED_FACE ( 'NONE', ( #9552 ), #14296, .F. ) ;
#1958 = PLANE ( 'NONE',  #13997 ) ;
#1959 = CARTESIAN_POINT ( 'NONE',  ( -84.02438362643999881, 99.17411849586700612, -152.4984795835769944 ) ) ;
#1960 = DIRECTION ( 'NONE',  ( -1.000000000000000000, 0.000000000000000000, 0.000000000000000000 ) ) ;
#1961 = VECTOR ( 'NONE', #5648, 1000.000000000000000 ) ;
#1962 = CYLINDRICAL_SURFACE ( 'NONE', #9589, 0.8000000000000113687 ) ;
#1963 = CARTESIAN_POINT ( 'NONE',  ( -73.64736697264743270, 75.17411849586699191, -44.99847958359794120 ) ) ;
#1964 = FACE_OUTER_BOUND ( 'NONE', #2098, .T. ) ;
#1965 = DIRECTION ( 'NONE',  ( -1.000000000000000000, 0.000000000000000000, 0.000000000000000000 ) ) ;
#1966 = ORIENTED_EDGE ( 'NONE', *, *, #10962, .T. ) ;
#1967 = CARTESIAN_POINT ( 'NONE',  ( 2.925834059445412638, -5.103531737064111340, -2.249496179459815615 ) ) ;
#1968 = VERTEX_POINT ( 'NONE', #14747 ) ;
#1969 = CARTESIAN_POINT ( 'NONE',  ( -15.50000000000000000, -0.4000000000000000222, 25.99999999999999645 ) ) ;
#1970 = EDGE_LOOP ( 'NONE', ( #6035, #5031, #9706, #12276 ) ) ;
#1971 = ORIENTED_EDGE ( 'NONE', *, *, #2292, .T. ) ;
#1972 = CARTESIAN_POINT ( 'NONE',  ( -1.183270876295518859, -2.296088562372991859, -3.904436448084174227 ) ) ;
#1973 = DIRECTION ( 'NONE',  ( 0.000000000000000000, 0.000000000000000000, 1.000000000000000000 ) ) ;
#1974 = FACE_OUTER_BOUND ( 'NONE', #5634, .T. ) ;
#1975 = APPLICATION_CONTEXT ( 'automotive_design' ) ;
#1976 = CARTESIAN_POINT ( 'NONE',  ( -73.01311196519618818, 67.29799558322736175, -83.44847958357698303 ) ) ;
#1977 = DIRECTION ( 'NONE',  ( -1.000000000000000000, 0.000000000000000000, 0.000000000000000000 ) ) ;
#1978 = CARTESIAN_POINT ( 'NONE',  ( 15.49557940054170047, -6.049654848385601793E-16, 18.93824625078692492 ) ) ;
#1979 = DIRECTION ( 'NONE',  ( 0.000000000000000000, -1.000000000000000000, -0.000000000000000000 ) ) ;
#1980 = DIRECTION ( 'NONE',  ( 1.000000000000000000, 0.000000000000000000, 0.000000000000000000 ) ) ;
#1981 = DIRECTION ( 'NONE',  ( 1.665334536937734811E-16, -4.340893464099163924E-16, 1.000000000000000000 ) ) ;
#1982 = ORIENTED_EDGE ( 'NONE', *, *, #15000, .F. ) ;
#1983 = CARTESIAN_POINT ( 'NONE',  ( -69.77438362644001302, 82.17411849586700612, -80.14847958357698587 ) ) ;
#1984 = CARTESIAN_POINT ( 'NONE',  ( 3.721607743032638638, -5.000000000000047073, 0.0009661164014421728431 ) ) ;
#1985 = ORIENTED_EDGE ( 'NONE', *, *, #4142, .T. ) ;
#1986 = CARTESIAN_POINT ( 'NONE',  ( -86.77438362644100778, 99.17411849586700612, -182.2484795835770228 ) ) ;
#1987 = LINE ( 'NONE', #744, #2404 ) ;
#1988 = CARTESIAN_POINT ( 'NONE',  ( 1.403561989263863629E-14, -5.500000000000003553, 0.000000000000000000 ) ) ;
#1989 = DIRECTION ( 'NONE',  ( -1.000000000000000000, 0.000000000000000000, 0.000000000000000000 ) ) ;
#1990 = CARTESIAN_POINT ( 'NONE',  ( 2.573385150445058223, -3.618985300545106920, 6.000000000000000000 ) ) ;
#1991 = CARTESIAN_POINT ( 'NONE',  ( -52.77438362643999881, 65.17411849586700612, -147.9984795835769944 ) ) ;
#1992 = EDGE_CURVE ( 'NONE', #7901, #1380, #5221, .T. ) ;
#1993 = DIRECTION ( 'NONE',  ( 1.000000000000000000, 0.000000000000000000, 0.000000000000000000 ) ) ;
#1994 = ORIENTED_EDGE ( 'NONE', *, *, #14565, .F. ) ;
#1995 = CARTESIAN_POINT ( 'NONE',  ( -104.2743836264399988, 111.1741184958670061, -79.49847958357700861 ) ) ;
#1996 = EDGE_CURVE ( 'NONE', #15166, #14071, #3972, .T. ) ;
#1997 = ORIENTED_EDGE ( 'NONE', *, *, #6881, .T. ) ;
#1998 = ORIENTED_EDGE ( 'NONE', *, *, #2383, .T. ) ;
#1999 = ORIENTED_EDGE ( 'NONE', *, *, #580, .T. ) ;
#2000 = ORIENTED_EDGE ( 'NONE', *, *, #7459, .T. ) ;
#2001 = EDGE_LOOP ( 'NONE', ( #728, #12873 ) ) ;
#2002 = AXIS2_PLACEMENT_3D ( 'NONE', #14613, #10183, #11207 ) ;
#2003 = CARTESIAN_POINT ( 'NONE',  ( -2.306523490862328885, -5.639838562372902153, 2.812621923907788091 ) ) ;
#2004 = CARTESIAN_POINT ( 'NONE',  ( 0.7459506331255062461, -1.366249999999944897, 3.755271276440939054 ) ) ;
#2005 = AXIS2_PLACEMENT_3D ( 'NONE', #14400, #11005, #6369 ) ;
#2006 = LINE ( 'NONE', #4264, #13282 ) ;
#2007 = CARTESIAN_POINT ( 'NONE',  ( -3.144577161339557669, -2.390624999999865885, -2.578777943664209982 ) ) ;
#2008 = DIRECTION ( 'NONE',  ( 0.9999934663667179313, -5.016628125758410379E-17, 0.003614861529251473839 ) ) ;
#2009 = PLANE ( 'NONE',  #10070 ) ;
#2010 = CARTESIAN_POINT ( 'NONE',  ( -69.77438362644001302, 82.17411849586700612, -150.4984795835769944 ) ) ;
#2011 = CARTESIAN_POINT ( 'NONE',  ( -4.166404709851690313, -1.484374999999892752, -0.4114723880711238513 ) ) ;
#2012 = CARTESIAN_POINT ( 'NONE',  ( -102.2743836264399988, 99.17411849586700612, -152.4984795835769944 ) ) ;
#2013 = EDGE_CURVE ( 'NONE', #9382, #10851, #1814, .T. ) ;
#2014 = CARTESIAN_POINT ( 'NONE',  ( 17.23697745638123280, 3.691760653673249681, -0.03314156585704653574 ) ) ;
#2015 = CARTESIAN_POINT ( 'NONE',  ( -50.27438362644099357, 99.17411849586700612, -79.59847958357700293 ) ) ;
#2016 = AXIS2_PLACEMENT_3D ( 'NONE', #14304, #14222, #1505 ) ;
#2017 = ORIENTED_EDGE ( 'NONE', *, *, #2580, .F. ) ;
#2018 = CARTESIAN_POINT ( 'NONE',  ( -77.52077156573416516, 60.67411849586702743, -79.59847958357700293 ) ) ;
#2019 = B_SPLINE_CURVE_WITH_KNOTS ( 'NONE', 3,
 ( #9090, #7930, #8235, #7162 ),
 .UNSPECIFIED., .F., .F.,
 ( 4, 4 ),
 ( 2.309401076757279912E-07, 0.002598307151460991539 ),
 .UNSPECIFIED. ) ;
#2020 = EDGE_CURVE ( 'NONE', #10091, #4114, #10233, .T. ) ;
#2021 = ORIENTED_EDGE ( 'NONE', *, *, #10725, .T. ) ;
#2022 = AXIS2_PLACEMENT_3D ( 'NONE', #12202, #14674, #13532 ) ;
#2023 = VERTEX_POINT ( 'NONE', #8930 ) ;
#2024 = EDGE_LOOP ( 'NONE', ( #13150, #5457, #12095, #8818 ) ) ;
#2025 = UNCERTAINTY_MEASURE_WITH_UNIT (LENGTH_MEASURE( 1.000000000000000082E-05 ), #8770, 'distance_accuracy_value', 'NONE');
#2026 = AXIS2_PLACEMENT_3D ( 'NONE', #6583, #8815, #12467 ) ;
#2027 = CARTESIAN_POINT ( 'NONE',  ( 16.33565937784172917, -0.3156604612126656106, 23.46090750622625976 ) ) ;
#2028 = CARTESIAN_POINT ( 'NONE',  ( -1.647113530155736916, -3.913124999999971099, -3.078783428963292490 ) ) ;
#2029 = EDGE_CURVE ( 'NONE', #12869, #8331, #13747, .T. ) ;
#2030 = CARTESIAN_POINT ( 'NONE',  ( -12.81835358098578403, 11.99999970914576330, -11.73358795631400397 ) ) ;
#2031 = EDGE_CURVE ( 'NONE', #7017, #12917, #7705, .T. ) ;
#2032 = CARTESIAN_POINT ( 'NONE',  ( -69.09337542095325091, 75.17411849586699191, -44.02377680093032097 ) ) ;
#2033 = DIRECTION ( 'NONE',  ( 0.000000000000000000, 0.000000000000000000, 1.000000000000000000 ) ) ;
#2034 = AXIS2_PLACEMENT_3D ( 'NONE', #9158, #11644, #6704 ) ;
#2035 = CARTESIAN_POINT ( 'NONE',  ( -15.50000000000000000, -5.000000000000000000, 22.50000000000000000 ) ) ;
#2036 = CARTESIAN_POINT ( 'NONE',  ( -2.773099908550811676, -0.4995676945082661580, 3.130259945877469363 ) ) ;
#2037 = LINE ( 'NONE', #1020, #12517 ) ;
#2038 = AXIS2_PLACEMENT_3D ( 'NONE', #10878, #13437, #14287 ) ;
#2039 = EDGE_CURVE ( 'NONE', #7102, #3975, #9641, .T. ) ;
#2040 = ORIENTED_EDGE ( 'NONE', *, *, #9155, .T. ) ;
#2041 = DIRECTION ( 'NONE',  ( -0.000000000000000000, -4.336808689942017736E-16, 1.000000000000000000 ) ) ;
#2042 = ADVANCED_FACE ( 'NONE', ( #13524 ), #5796, .T. ) ;
#2043 = ORIENTED_EDGE ( 'NONE', *, *, #2020, .T. ) ;
#2044 = EDGE_CURVE ( 'NONE', #10133, #13729, #2806, .T. ) ;
#2045 = ORIENTED_EDGE ( 'NONE', *, *, #13227, .T. ) ;
#2046 = CYLINDRICAL_SURFACE ( 'NONE', #13670, 1.500000000000001332 ) ;
#2047 = ORIENTED_EDGE ( 'NONE', *, *, #12073, .T. ) ;
#2048 = B_SPLINE_CURVE_WITH_KNOTS ( 'NONE', 3,
 ( #11751, #3374, #2439, #7258, #6947, #4698, #8180, #10416, #14147, #9260, #14224, #13998 ),
 .UNSPECIFIED., .F., .F.,
 ( 4, 2, 2, 2, 2, 4 ),
 ( 2.544323688695603672E-07, 0.001342108318545691186, 0.002013035261634101361, 0.002683962204722511753, 0.004025816090899332102, 0.005367669977076152885 ),
 .UNSPECIFIED. ) ;
#2049 = ORIENTED_EDGE ( 'NONE', *, *, #13972, .F. ) ;
#2050 = CIRCLE ( 'NONE', #813, 3.000000000000002665 ) ;
#2051 = CARTESIAN_POINT ( 'NONE',  ( 2.831777009049577298, -2.874213562372941677, 2.829717318554673788 ) ) ;
#2052 = EDGE_CURVE ( 'NONE', #9286, #14331, #10155, .T. ) ;
#2053 = CARTESIAN_POINT ( 'NONE',  ( 15.50000000000000000, -1.037157890325000054, 22.50000000000000000 ) ) ;
#2054 = CARTESIAN_POINT ( 'NONE',  ( 15.50000000000000000, -0.4000000000005274892, -22.50000000000000000 ) ) ;
#2055 = DIRECTION ( 'NONE',  ( 0.000000000000000000, 1.387778780781444413E-14, -1.000000000000000000 ) ) ;
#2056 = ADVANCED_FACE ( 'NONE', ( #7638 ), #11181, .T. ) ;
#2057 = CYLINDRICAL_SURFACE ( 'NONE', #13482, 2.750000000000002665 ) ;
#2058 = DIRECTION ( 'NONE',  ( 1.000000000000000000, 0.000000000000000000, 0.000000000000000000 ) ) ;
#2059 = AXIS2_PLACEMENT_3D ( 'NONE', #4055, #8782, #9383 ) ;
#2060 = FACE_OUTER_BOUND ( 'NONE', #6283, .T. ) ;
#2061 = APPLICATION_PROTOCOL_DEFINITION ( 'draft international standard', 'automotive_design', 1998, #8332 ) ;
#2062 = VERTEX_POINT ( 'NONE', #13668 ) ;
#2063 = VECTOR ( 'NONE', #3488, 1000.000000000000000 ) ;
#2064 = CARTESIAN_POINT ( 'NONE',  ( 3.756292859848885168, -0.6318749999998841682, -1.140955529460069950 ) ) ;
#2065 = EDGE_LOOP ( 'NONE', ( #2140, #3233, #8362, #2049 ) ) ;
#2066 = CARTESIAN_POINT ( 'NONE',  ( -1.090659875871078599, -1.881874999999897824, -3.598793876473114661 ) ) ;
#2067 = VECTOR ( 'NONE', #2260, 1000.000000000000000 ) ;
#2068 = CARTESIAN_POINT ( 'NONE',  ( -52.77438362643999881, 62.81621999649657084, -150.4984795835770228 ) ) ;
#2069 = AXIS2_PLACEMENT_3D ( 'NONE', #8203, #5589, #5671 ) ;
#2070 = CARTESIAN_POINT ( 'NONE',  ( 3.953167801354152022, -0.4995676945082486720, 0.3853396878248828150 ) ) ;
#2071 = FACE_OUTER_BOUND ( 'NONE', #12830, .T. ) ;
#2072 = DIRECTION ( 'NONE',  ( 0.000000000000000000, 0.000000000000000000, 1.000000000000000000 ) ) ;
#2073 = ORIENTED_EDGE ( 'NONE', *, *, #4785, .T. ) ;
#2074 = CARTESIAN_POINT ( 'NONE',  ( -86.77438362643999881, 65.17411849586700612, -150.4984795835770228 ) ) ;
#2075 = VECTOR ( 'NONE', #2569, 999.9999999999998863 ) ;
#2076 = VECTOR ( 'NONE', #5809, 1000.000000000000000 ) ;
#2077 = ORIENTED_EDGE ( 'NONE', *, *, #13386, .F. ) ;
#2078 = VERTEX_POINT ( 'NONE', #5386 ) ;
#2079 = CARTESIAN_POINT ( 'NONE',  ( -3.406603204915187533, -4.053749999999936016, -0.6763000812039869913 ) ) ;
#2080 = ORIENTED_EDGE ( 'NONE', *, *, #607, .F. ) ;
#2081 = ORIENTED_EDGE ( 'NONE', *, *, #2104, .F. ) ;
#2082 = EDGE_LOOP ( 'NONE', ( #9067, #9804, #5693, #973 ) ) ;
#2083 = CARTESIAN_POINT ( 'NONE',  ( -3.385045168076599165, -5.436713562373150843, -1.403157895329555593 ) ) ;
#2084 = CARTESIAN_POINT ( 'NONE',  ( -2.814361612698371928, -0.2100000000001143730, 2.816411668391514578 ) ) ;
#2085 = CARTESIAN_POINT ( 'NONE',  ( 1.161840668242749786, -5.408364452671047928, 3.095256225502303948 ) ) ;
#2086 = CARTESIAN_POINT ( 'NONE',  ( 1.163914675889782702, -2.796875000000069722, 3.840555497293599352 ) ) ;
#2087 = CARTESIAN_POINT ( 'NONE',  ( -46.58670980944423690, 0.000000000000000000, 89.50956111919107627 ) ) ;
#2088 = EDGE_CURVE ( 'NONE', #9247, #7059, #485, .T. ) ;
#2089 = VECTOR ( 'NONE', #3773, 1000.000000000000000 ) ;
#2090 = CARTESIAN_POINT ( 'NONE',  ( 1.634139617129772404, 11.99999970914575798, -0.3335879563140091153 ) ) ;
#2091 = LINE ( 'NONE', #1943, #6900 ) ;
#2092 = DIRECTION ( 'NONE',  ( 0.000000000000000000, 0.000000000000000000, 1.000000000000000000 ) ) ;
#2093 = DIRECTION ( 'NONE',  ( 0.000000000000000000, 0.000000000000000000, -1.000000000000000000 ) ) ;
#2094 = CARTESIAN_POINT ( 'NONE',  ( -42.77438362644000591, 104.6741184958670061, -152.4984795835769944 ) ) ;
#2095 = ORIENTED_EDGE ( 'NONE', *, *, #7161, .T. ) ;
#2096 = CARTESIAN_POINT ( 'NONE',  ( -69.77438362644001302, 94.57411849586699759, -89.99847958357699440 ) ) ;
#2097 = EDGE_LOOP ( 'NONE', ( #13143, #668, #3903, #9455 ) ) ;
#2098 = EDGE_LOOP ( 'NONE', ( #5281, #776, #370, #7535 ) ) ;
#2099 = VERTEX_POINT ( 'NONE', #1873 ) ;
#2100 = TOROIDAL_SURFACE ( 'NONE', #3594, 2.700000000000000178, 0.2000000000000000111 ) ;
#2101 = VECTOR ( 'NONE', #5397, 1000.000000000000000 ) ;
#2102 = LINE ( 'NONE', #6852, #3272 ) ;
#2103 = VECTOR ( 'NONE', #14131, 1000.000000000000000 ) ;
#2104 = EDGE_CURVE ( 'NONE', #9860, #10234, #9737, .T. ) ;
#2105 = CARTESIAN_POINT ( 'NONE',  ( -2.874539946219666575, -4.178749999999989306, 1.919644203647528302 ) ) ;
#2106 = FACE_OUTER_BOUND ( 'NONE', #919, .T. ) ;
#2107 = DIRECTION ( 'NONE',  ( -0.000000000000000000, -0.000000000000000000, 1.000000000000000000 ) ) ;
#2108 = CARTESIAN_POINT ( 'NONE',  ( 21.98164641901421135, -3.654316742536411589, 0.2664120436859909735 ) ) ;
#2109 = DIRECTION ( 'NONE',  ( -0.000000000000000000, -0.000000000000000000, 1.000000000000000000 ) ) ;
#2110 = LINE ( 'NONE', #5855, #13817 ) ;
#2111 = DIRECTION ( 'NONE',  ( 0.1802821511763431361, 0.1220014872200674283, -0.9760194583528146728 ) ) ;
#2112 = MECHANICAL_DESIGN_GEOMETRIC_PRESENTATION_REPRESENTATION (  '', ( #8805 ), #4597 ) ;
#2113 = DIRECTION ( 'NONE',  ( 0.000000000000000000, 0.000000000000000000, -1.000000000000000000 ) ) ;
#2114 = VECTOR ( 'NONE', #10222, 1000.000000000000000 ) ;
#2115 = ORIENTED_EDGE ( 'NONE', *, *, #5726, .T. ) ;
#2116 = AXIS2_PLACEMENT_3D ( 'NONE', #14941, #2942, #6600 ) ;
#2117 = FACE_BOUND ( 'NONE', #14397, .T. ) ;
#2118 = ORIENTED_EDGE ( 'NONE', *, *, #10917, .F. ) ;
#2119 = EDGE_LOOP ( 'NONE', ( #5408, #8599, #371, #12111 ) ) ;
#2120 = DIRECTION ( 'NONE',  ( -1.000000000000000000, 0.000000000000000000, 0.000000000000000000 ) ) ;
#2121 = EDGE_LOOP ( 'NONE', ( #11341, #8950, #258, #8862 ) ) ;
#2122 = CARTESIAN_POINT ( 'NONE',  ( -2.641694630006354405, -1.640624999999979572, 3.221290409975102520 ) ) ;
#2123 = VERTEX_POINT ( 'NONE', #5455 ) ;
#2124 = COLOUR_RGB ( '', 0.08235294, 0.09019608, 0.10196078) ;
#2125 = EDGE_CURVE ( 'NONE', #6527, #6505, #1433, .T. ) ;
#2126 = CARTESIAN_POINT ( 'NONE',  ( -0.7860821048245157927, -2.717963562373058473, 3.946463394123028490 ) ) ;
#2127 = AXIS2_PLACEMENT_3D ( 'NONE', #13772, #3147, #7880 ) ;
#2128 = CONICAL_SURFACE ( 'NONE', #6616, 3.173335668876520632, 0.9162978572970248425 ) ;
#2129 = CARTESIAN_POINT ( 'NONE',  ( -9.503456061879928640, -12.00000029085427222, 69.60114695342350899 ) ) ;
#2130 = FACE_OUTER_BOUND ( 'NONE', #9678, .T. ) ;
#2131 = EDGE_CURVE ( 'NONE', #4691, #4583, #814, .T. ) ;
#2132 = DIRECTION ( 'NONE',  ( 0.000000000000000000, 0.000000000000000000, 1.000000000000000000 ) ) ;
#2133 = CARTESIAN_POINT ( 'NONE',  ( -52.77438362644000591, 82.17411849586700612, -79.59847958357700293 ) ) ;
#2134 = AXIS2_PLACEMENT_3D ( 'NONE', #272, #5109, #13480 ) ;
#2135 = CARTESIAN_POINT ( 'NONE',  ( 10.10045295220800554, -11.00000029085428110, 70.08978589960025829 ) ) ;
#2136 = CARTESIAN_POINT ( 'NONE',  ( -15.50000000000000000, 998.9628421096749662, 22.50000000000000000 ) ) ;
#2137 = VECTOR ( 'NONE', #1016, 1000.000000000000000 ) ;
#2138 = EDGE_CURVE ( 'NONE', #13430, #14951, #5047, .T. ) ;
#2139 = AXIS2_PLACEMENT_3D ( 'NONE', #2254, #5931, #14125 ) ;
#2140 = ORIENTED_EDGE ( 'NONE', *, *, #11227, .T. ) ;
#2141 = CARTESIAN_POINT ( 'NONE',  ( -3.640012805681923869, -5.484374212848019958, -0.3571734599629662332 ) ) ;
#2142 = ORIENTED_EDGE ( 'NONE', *, *, #7330, .F. ) ;
#2143 = EDGE_CURVE ( 'NONE', #8110, #10442, #14120, .T. ) ;
#2144 = CIRCLE ( 'NONE', #11822, 0.6000000000000000888 ) ;
#2145 = CARTESIAN_POINT ( 'NONE',  ( -3.581969766213484174, -3.100624999999847198, 0.3518610084922548231 ) ) ;
#2146 = FACE_BOUND ( 'NONE', #573, .T. ) ;
#2147 = EDGE_CURVE ( 'NONE', #7923, #11451, #6921, .T. ) ;
#2148 = VECTOR ( 'NONE', #848, 1000.000000000000000 ) ;
#2149 = FACE_OUTER_BOUND ( 'NONE', #13147, .T. ) ;
#2150 = DIRECTION ( 'NONE',  ( 1.000000000000000000, 0.000000000000000000, 0.000000000000000000 ) ) ;
#2151 = DIRECTION ( 'NONE',  ( 0.000000000000000000, 1.000000000000000000, 0.000000000000000000 ) ) ;
#2152 = CARTESIAN_POINT ( 'NONE',  ( -54.81638362644100226, 100.3530677455522238, -147.9984795835769944 ) ) ;
#2153 = ORIENTED_EDGE ( 'NONE', *, *, #14095, .T. ) ;
#2154 = DIRECTION ( 'NONE',  ( 0.9848077530122082424, 0.1736481776669299149, 0.000000000000000000 ) ) ;
#2155 = ORIENTED_EDGE ( 'NONE', *, *, #10470, .F. ) ;
#2156 = AXIS2_PLACEMENT_3D ( 'NONE', #15240, #2293, #4552 ) ;
#2157 = ORIENTED_EDGE ( 'NONE', *, *, #4679, .F. ) ;
#2158 = EDGE_LOOP ( 'NONE', ( #8629, #9535, #10726, #7373 ) ) ;
#2159 = ORIENTED_EDGE ( 'NONE', *, *, #14425, .T. ) ;
#2160 = ORIENTED_EDGE ( 'NONE', *, *, #7553, .T. ) ;
#2161 = CARTESIAN_POINT ( 'NONE',  ( 2.762998497935824194, -6.108588562373387987, -2.269244778944577323 ) ) ;
#2162 = CARTESIAN_POINT ( 'NONE',  ( -2.135074830120813782, -1.241249999999904707, 3.197897516496418291 ) ) ;
#2163 = CARTESIAN_POINT ( 'NONE',  ( 3.325473450044490242, -2.906249999999835243, 2.220260485081660740 ) ) ;
#2164 = CARTESIAN_POINT ( 'NONE',  ( 14.25000000000000000, -2.500000000000000000, 21.77831216351300014 ) ) ;
#2165 = FACE_OUTER_BOUND ( 'NONE', #2197, .T. ) ;
#2166 = AXIS2_PLACEMENT_3D ( 'NONE', #11885, #12122, #1492 ) ;
#2167 = FACE_OUTER_BOUND ( 'NONE', #6971, .T. ) ;
#2168 = LINE ( 'NONE', #7071, #2279 ) ;
#2169 = DIRECTION ( 'NONE',  ( 0.000000000000000000, 0.000000000000000000, -1.000000000000000000 ) ) ;
#2170 = CARTESIAN_POINT ( 'NONE',  ( -9.797174393178965434E-17, 9.500000000000000000, 0.000000000000000000 ) ) ;
#2171 = DIRECTION ( 'NONE',  ( 0.000000000000000000, 0.000000000000000000, 1.000000000000000000 ) ) ;
#2172 = ORIENTED_EDGE ( 'NONE', *, *, #13987, .F. ) ;
#2173 = CARTESIAN_POINT ( 'NONE',  ( -89.27438362643999881, 65.17411849586700612, -145.2984795835770058 ) ) ;
#2174 = ORIENTED_EDGE ( 'NONE', *, *, #3354, .T. ) ;
#2175 = ORIENTED_EDGE ( 'NONE', *, *, #11010, .F. ) ;
#2176 = ORIENTED_EDGE ( 'NONE', *, *, #6800, .F. ) ;
#2177 = EDGE_CURVE ( 'NONE', #13870, #11017, #9224, .T. ) ;
#2178 =( REPRESENTATION_RELATIONSHIP ('NONE','NONE', #13541, #2929 ) REPRESENTATION_RELATIONSHIP_WITH_TRANSFORMATION ( #7657 )SHAPE_REPRESENTATION_RELATIONSHIP( ) );
#2179 = AXIS2_PLACEMENT_3D ( 'NONE', #14406, #11791, #8379 ) ;
#2180 = DIRECTION ( 'NONE',  ( 0.000000000000000000, 0.000000000000000000, 1.000000000000000000 ) ) ;
#2181 = CARTESIAN_POINT ( 'NONE',  ( -1.318845896519720284, -4.272500000000155396, 3.181678407182404023 ) ) ;
#2182 = CARTESIAN_POINT ( 'NONE',  ( -16.54633693294649888, -0.2717122460102565085, -23.33927276307431598 ) ) ;
#2183 = DIRECTION ( 'NONE',  ( -1.000000000000000000, 0.000000000000000000, 0.000000000000000000 ) ) ;
#2184 = CARTESIAN_POINT ( 'NONE',  ( -69.77438362644001302, 82.17411849586700612, -80.44847958357698303 ) ) ;
#2185 = CARTESIAN_POINT ( 'NONE',  ( 0.000000000000000000, 0.000000000000000000, 6.000000000000000000 ) ) ;
#2186 = CARTESIAN_POINT ( 'NONE',  ( -52.77438362644000591, 99.17411849586700612, -86.49847958357699440 ) ) ;
#2187 = DIRECTION ( 'NONE',  ( -1.000000000000000000, 0.000000000000000000, -0.000000000000000000 ) ) ;
#2188 = DIRECTION ( 'NONE',  ( 0.000000000000000000, 0.000000000000000000, -1.000000000000000000 ) ) ;
#2189 = CARTESIAN_POINT ( 'NONE',  ( -69.77438362644001302, 82.17411849586700612, -80.14847958357698587 ) ) ;
#2190 = AXIS2_PLACEMENT_3D ( 'NONE', #4181, #2941, #12103 ) ;
#2191 = ORIENTED_EDGE ( 'NONE', *, *, #5274, .T. ) ;
#2192 = LINE ( 'NONE', #9473, #3647 ) ;
#2193 = EDGE_CURVE ( 'NONE', #2946, #9156, #3355, .T. ) ;
#2194 = VERTEX_POINT ( 'NONE', #15044 ) ;
#2195 = ORIENTED_EDGE ( 'NONE', *, *, #4021, .T. ) ;
#2196 = CARTESIAN_POINT ( 'NONE',  ( -75.01311196519617397, 67.29799558322736175, -83.44847958357698303 ) ) ;
#2197 = EDGE_LOOP ( 'NONE', ( #4531, #2968, #2811, #2542, #7497, #9058, #12496 ) ) ;
#2198 = EDGE_CURVE ( 'NONE', #15131, #10091, #10388, .T. ) ;
#2199 = CARTESIAN_POINT ( 'NONE',  ( -4.100362740845592491, -1.531249999999860556, 0.8144810970459482879 ) ) ;
#2200 = ORIENTED_EDGE ( 'NONE', *, *, #15107, .F. ) ;
#2201 = CARTESIAN_POINT ( 'NONE',  ( 3.622844214532213503, -2.077338562372990527, -1.938139479208375038 ) ) ;
#2202 = CIRCLE ( 'NONE', #15069, 2.500000000000002220 ) ;
#2203 = CYLINDRICAL_SURFACE ( 'NONE', #2757, 2.000000000000001776 ) ;
#2204 = CARTESIAN_POINT ( 'NONE',  ( -104.2743836264399988, 60.67411849586700612, -67.49847958357700861 ) ) ;
#2205 = DIRECTION ( 'NONE',  ( 1.000000000000000000, 0.000000000000000000, 0.000000000000000000 ) ) ;
#2206 = CARTESIAN_POINT ( 'NONE',  ( 2.573385150445058223, -19.31989681812820692, 0.000000000000000000 ) ) ;
#2207 = ORIENTED_EDGE ( 'NONE', *, *, #14548, .F. ) ;
#2208 = FACE_OUTER_BOUND ( 'NONE', #13929, .T. ) ;
#2209 = EDGE_CURVE ( 'NONE', #6162, #6907, #7280, .T. ) ;
#2210 = CARTESIAN_POINT ( 'NONE',  ( -50.73238362644099197, 97.99516924618178848, -150.4984795835770228 ) ) ;
#2211 = ORIENTED_EDGE ( 'NONE', *, *, #2902, .F. ) ;
#2212 = ADVANCED_FACE ( 'NONE', ( #3338, #3256 ), #2328, .T. ) ;
#2213 = CARTESIAN_POINT ( 'NONE',  ( 3.931950937192210116, -0.5849999999998678479, -0.001434051515494263150 ) ) ;
#2214 = VERTEX_POINT ( 'NONE', #2018 ) ;
#2215 = CARTESIAN_POINT ( 'NONE',  ( -3.093239089446854884, -2.178749999999916476, 2.068481483294962953 ) ) ;
#2216 = CARTESIAN_POINT ( 'NONE',  ( -1.006616814747114486E-29, -2.568816543514388222E-44, -4.500000000000000888 ) ) ;
#2217 = ADVANCED_FACE ( 'NONE', ( #11797 ), #12651, .F. ) ;
#2218 = ADVANCED_FACE ( 'NONE', ( #7990 ), #1006, .T. ) ;
#2219 = CARTESIAN_POINT ( 'NONE',  ( -50.73238362643999722, 66.35306774555222376, -147.9984795835769944 ) ) ;
#2220 = DIRECTION ( 'NONE',  ( 1.000000000000000000, 0.000000000000000000, 1.224646799147353454E-16 ) ) ;
#2221 = CARTESIAN_POINT ( 'NONE',  ( -12.81835358098578403, -12.00000029085423670, -14.13358795631400611 ) ) ;
#2222 = CARTESIAN_POINT ( 'NONE',  ( 17.04394838817069768, -11.40000029085424238, 0.2824263826447100945 ) ) ;
#2223 = EDGE_CURVE ( 'NONE', #4691, #4583, #8070, .T. ) ;
#2224 = LINE ( 'NONE', #11691, #10195 ) ;
#2225 = EDGE_LOOP ( 'NONE', ( #13748, #10679 ) ) ;
#2226 = DIRECTION ( 'NONE',  ( 0.000000000000000000, 0.000000000000000000, -1.000000000000000000 ) ) ;
#2227 = ORIENTED_EDGE ( 'NONE', *, *, #7968, .F. ) ;
#2228 = EDGE_CURVE ( 'NONE', #1792, #11018, #6049, .T. ) ;
#2229 = ORIENTED_EDGE ( 'NONE', *, *, #6903, .T. ) ;
#2230 = CARTESIAN_POINT ( 'NONE',  ( -2.669536895096369378, -4.194375000000057696, 2.192493760422842719 ) ) ;
#2231 = ORIENTED_EDGE ( 'NONE', *, *, #3280, .F. ) ;
#2232 = ORIENTED_EDGE ( 'NONE', *, *, #7566, .T. ) ;
#2233 = VERTEX_POINT ( 'NONE', #4505 ) ;
#2234 = CARTESIAN_POINT ( 'NONE',  ( 3.646332799887131770, -5.030463562373060249, -0.7266944397774037778 ) ) ;
#2235 = DIRECTION ( 'NONE',  ( 0.7071067811865525687, -0.000000000000000000, -0.7071067811865425767 ) ) ;
#2236 = DIRECTION ( 'NONE',  ( 0.4999999999999999445, 0.000000000000000000, -0.8660254037844387076 ) ) ;
#2237 = LINE ( 'NONE', #7911, #4287 ) ;
#2238 = DIRECTION ( 'NONE',  ( -0.9961946980917452121, 0.000000000000000000, -0.08715574274766160756 ) ) ;
#2239 = CARTESIAN_POINT ( 'NONE',  ( -15.50000000000000000, -0.4000000000000000222, -25.99999999999999645 ) ) ;
#2240 = DIRECTION ( 'NONE',  ( 0.000000000000000000, 1.000000000000000000, 0.000000000000000000 ) ) ;
#2241 = CARTESIAN_POINT ( 'NONE',  ( -16.75000000000000000, -0.2038245569916330158, 21.77831216351300014 ) ) ;
#2242 = DIRECTION ( 'NONE',  ( 0.000000000000000000, 0.000000000000000000, -1.000000000000000000 ) ) ;
#2243 = ADVANCED_FACE ( 'NONE', ( #7920 ), #6769, .F. ) ;
#2244 = CARTESIAN_POINT ( 'NONE',  ( -3.322613055092911161, -5.069375000000116316, -0.3280989749989032256 ) ) ;
#2245 = LINE ( 'NONE', #4819, #14938 ) ;
#2246 = ORIENTED_EDGE ( 'NONE', *, *, #1948, .T. ) ;
#2247 = CYLINDRICAL_SURFACE ( 'NONE', #4789, 1.785937500000001066 ) ;
#2248 = ORIENTED_EDGE ( 'NONE', *, *, #8490, .F. ) ;
#2249 = CIRCLE ( 'NONE', #12908, 5.500000000000005329 ) ;
#2250 = ORIENTED_EDGE ( 'NONE', *, *, #6853, .F. ) ;
#2251 = VERTEX_POINT ( 'NONE', #2173 ) ;
#2252 =( NAMED_UNIT ( * ) SI_UNIT ( $, .STERADIAN. ) SOLID_ANGLE_UNIT ( ) );
#2253 = CARTESIAN_POINT ( 'NONE',  ( -1.914696782014857490, -4.241249999999832987, 2.867854448260447775 ) ) ;
#2254 = CARTESIAN_POINT ( 'NONE',  ( -69.77438362644001302, 82.17411849586700612, -82.44847958357698303 ) ) ;
#2255 = DIRECTION ( 'NONE',  ( -1.000000000000000000, 0.000000000000000000, 0.000000000000000000 ) ) ;
#2256 = DIRECTION ( 'NONE',  ( -0.000000000000000000, -1.000000000000000000, -0.000000000000000000 ) ) ;
#2257 = DIRECTION ( 'NONE',  ( -1.284980352575412699E-16, 0.000000000000000000, -1.000000000000000000 ) ) ;
#2258 = AXIS2_PLACEMENT_3D ( 'NONE', #11439, #804, #9105 ) ;
#2259 = PLANE ( 'NONE',  #7881 ) ;
#2260 = DIRECTION ( 'NONE',  ( 0.8660254037844387076, 0.4999999999999998890, 0.000000000000000000 ) ) ;
#2261 = PLANE ( 'NONE',  #6343 ) ;
#2262 = LINE ( 'NONE', #5778, #11970 ) ;
#2263 = CONICAL_SURFACE ( 'NONE', #13917, 4.500000000000000888, 1.396263401595466691 ) ;
#2264 = EDGE_LOOP ( 'NONE', ( #2000, #5533, #4670, #12676 ) ) ;
#2265 = CARTESIAN_POINT ( 'NONE',  ( -86.77438362644100778, 96.81621999649657084, -147.9984795835769944 ) ) ;
#2266 = ORIENTED_EDGE ( 'NONE', *, *, #14266, .T. ) ;
#2267 = ORIENTED_EDGE ( 'NONE', *, *, #2486, .T. ) ;
#2268 = CARTESIAN_POINT ( 'NONE',  ( -16.75000000000000000, -0.2038245569916330158, -23.22168783648699986 ) ) ;
#2269 = ORIENTED_EDGE ( 'NONE', *, *, #4403, .T. ) ;
#2270 = VECTOR ( 'NONE', #9483, 1000.000000000000000 ) ;
#2271 = CARTESIAN_POINT ( 'NONE',  ( 1.991706217211437036, -1.171874999999983347, -3.729459312589495923 ) ) ;
#2272 = EDGE_LOOP ( 'NONE', ( #3211, #14496, #5735, #11583 ) ) ;
#2273 = CARTESIAN_POINT ( 'NONE',  ( -3.884733793026120541, -2.452338562373202802, -1.176880867913740358 ) ) ;
#2274 = DIRECTION ( 'NONE',  ( 4.710339085808869774E-17, 1.000000000000000000, -1.047133521511407648E-16 ) ) ;
#2275 = VECTOR ( 'NONE', #6662, 1000.000000000000000 ) ;
#2276 = DIRECTION ( 'NONE',  ( 1.000000000000000000, 0.000000000000000000, -0.000000000000000000 ) ) ;
#2277 = DIRECTION ( 'NONE',  ( -1.000000000000000000, 0.000000000000000000, 0.000000000000000000 ) ) ;
#2278 = ADVANCED_FACE ( 'NONE', ( #5760 ), #2247, .F. ) ;
#2279 = VECTOR ( 'NONE', #2240, 1000.000000000000000 ) ;
#2280 = DIRECTION ( 'NONE',  ( 0.000000000000000000, 0.000000000000000000, 1.000000000000000000 ) ) ;
#2281 = ORIENTED_EDGE ( 'NONE', *, *, #13625, .F. ) ;
#2282 = CARTESIAN_POINT ( 'NONE',  ( 2.937061643673781752, -5.103115294876279684, -2.234448363260541193 ) ) ;
#2283 = DIRECTION ( 'NONE',  ( 0.000000000000000000, 0.000000000000000000, 1.000000000000000000 ) ) ;
#2284 = AXIS2_PLACEMENT_3D ( 'NONE', #8969, #6731, #10271 ) ;
#2285 = SHAPE_DEFINITION_REPRESENTATION ( #13060, #6613 ) ;
#2286 = ORIENTED_EDGE ( 'NONE', *, *, #2428, .T. ) ;
#2287 = PRESENTATION_STYLE_ASSIGNMENT (( #4466 ) ) ;
#2288 = CARTESIAN_POINT ( 'NONE',  ( 2.769370807496426945, -0.7100000000000333822, -2.767918543042355850 ) ) ;
#2289 = ORIENTED_EDGE ( 'NONE', *, *, #13237, .F. ) ;
#2290 = CARTESIAN_POINT ( 'NONE',  ( 1.096135970525389913, -1.788124999999989750, -3.610092524386871560 ) ) ;
#2291 = LINE ( 'NONE', #7042, #13893 ) ;
#2292 = EDGE_CURVE ( 'NONE', #9398, #2214, #13224, .T. ) ;
#2293 = DIRECTION ( 'NONE',  ( 0.000000000000000000, 1.000000000000000000, 0.000000000000000000 ) ) ;
#2294 = VECTOR ( 'NONE', #13514, 1000.000000000000000 ) ;
#2295 = CARTESIAN_POINT ( 'NONE',  ( -77.52077156573416516, 110.1741184958670061, -15.85886927678779834 ) ) ;
#2296 = AXIS2_PLACEMENT_3D ( 'NONE', #9454, #3721, #1314 ) ;
#2297 = PLANE ( 'NONE',  #9124 ) ;
#2298 = DIRECTION ( 'NONE',  ( 0.000000000000000000, 0.000000000000000000, 1.000000000000000000 ) ) ;
#2299 = CARTESIAN_POINT ( 'NONE',  ( -52.77438362644000591, 99.17411849586700612, -152.4984795835769944 ) ) ;
#2300 = AXIS2_PLACEMENT_3D ( 'NONE', #4167, #1908, #10191 ) ;
#2301 = EDGE_LOOP ( 'NONE', ( #7615, #9042, #6247, #1625 ) ) ;
#2302 = CARTESIAN_POINT ( 'NONE',  ( 23.25000000000000000, -10.00000000000000000, 27.00000000000000000 ) ) ;
#2303 = VERTEX_POINT ( 'NONE', #6995 ) ;
#2304 = EDGE_CURVE ( 'NONE', #14968, #1927, #3801, .T. ) ;
#2305 = ORIENTED_EDGE ( 'NONE', *, *, #3996, .T. ) ;
#2306 = CARTESIAN_POINT ( 'NONE',  ( 0.001278483876778065912, -4.335000000000164277, 3.435880605283331946 ) ) ;
#2307 = ORIENTED_EDGE ( 'NONE', *, *, #5092, .F. ) ;
#2308 = EDGE_LOOP ( 'NONE', ( #8118, #3549, #10138, #7854 ) ) ;
#2309 = VECTOR ( 'NONE', #4461, 1000.000000000000114 ) ;
#2310 = AXIS2_PLACEMENT_3D ( 'NONE', #6451, #11014, #13724 ) ;
#2311 = ORIENTED_EDGE ( 'NONE', *, *, #3453, .F. ) ;
#2312 = CARTESIAN_POINT ( 'NONE',  ( 2.080555833684100797, -4.842963562373058473, 3.111297368939876407 ) ) ;
#2313 = DIRECTION ( 'NONE',  ( -0.000000000000000000, -0.000000000000000000, 1.000000000000000000 ) ) ;
#2314 = EDGE_CURVE ( 'NONE', #5254, #877, #14414, .T. ) ;
#2315 = CIRCLE ( 'NONE', #574, 0.8000000000000176970 ) ;
#2316 = CARTESIAN_POINT ( 'NONE',  ( -2.598076211353319120, 1.678847577293364424, 4.500000000000000888 ) ) ;
#2317 = CARTESIAN_POINT ( 'NONE',  ( 66.41329019055577021, 0.000000000000000000, 89.50956111919107627 ) ) ;
#2318 = DIRECTION ( 'NONE',  ( 0.000000000000000000, 1.000000000000000000, 0.000000000000000000 ) ) ;
#2319 = ADVANCED_FACE ( 'NONE', ( #11948 ), #11732, .F. ) ;
#2320 = EDGE_CURVE ( 'NONE', #9847, #9368, #13948, .T. ) ;
#2321 = CARTESIAN_POINT ( 'NONE',  ( 21.98164641901421135, -11.40000029085423705, -8.183940086454239093 ) ) ;
#2322 = CARTESIAN_POINT ( 'NONE',  ( 3.469446951953614189E-15, -24.00000000000000000, 6.000000000000000000 ) ) ;
#2323 = VECTOR ( 'NONE', #14603, 1000.000000000000114 ) ;
#2324 = CIRCLE ( 'NONE', #11004, 8.050000000000000711 ) ;
#2325 = CARTESIAN_POINT ( 'NONE',  ( -3.196762997434627440, -4.147500000000007958, 1.325534829466321840 ) ) ;
#2326 = DIRECTION ( 'NONE',  ( 0.000000000000000000, 0.000000000000000000, -1.000000000000000000 ) ) ;
#2327 = ORIENTED_EDGE ( 'NONE', *, *, #12472, .F. ) ;
#2328 = PLANE ( 'NONE',  #5036 ) ;
#2329 = EDGE_CURVE ( 'NONE', #469, #6326, #8530, .T. ) ;
#2330 = ORIENTED_EDGE ( 'NONE', *, *, #15085, .F. ) ;
#2331 = ORIENTED_EDGE ( 'NONE', *, *, #7272, .T. ) ;
#2332 = DIRECTION ( 'NONE',  ( -0.000000000000000000, -0.000000000000000000, 1.000000000000000000 ) ) ;
#2333 = CLOSED_SHELL ( 'NONE', ( #11664, #4399, #12367, #12302, #7256, #5871, #621, #2702, #12849, #14914, #5915, #7560, #7065, #8954, #10860 ) ) ;
#2334 = VECTOR ( 'NONE', #473, 1000.000000000000000 ) ;
#2335 = CARTESIAN_POINT ( 'NONE',  ( 2.024885806073651651, -2.741249999999974207, -3.032875982375832891 ) ) ;
#2336 = CIRCLE ( 'NONE', #6566, 2.500000000000002220 ) ;
#2337 = EDGE_CURVE ( 'NONE', #8985, #8702, #8988, .T. ) ;
#2338 = CARTESIAN_POINT ( 'NONE',  ( 15.29686605390242704, -0.2715358723600077573, 21.17390376548697972 ) ) ;
#2339 = CARTESIAN_POINT ( 'NONE',  ( 2.372013019084901586, -4.859374999999952927, 2.891838320553053343 ) ) ;
#2340 = DIRECTION ( 'NONE',  ( 1.000000000000000000, 1.727704675731647582E-15, 0.000000000000000000 ) ) ;
#2341 = DIRECTION ( 'NONE',  ( 0.000000000000000000, 1.000000000000000000, 0.000000000000000000 ) ) ;
#2342 = CARTESIAN_POINT ( 'NONE',  ( 10.10406781373725771, 10.99999970914572778, 70.08979243323354069 ) ) ;
#2343 = PLANE ( 'NONE',  #8757 ) ;
#2344 = FACE_BOUND ( 'NONE', #12322, .T. ) ;
#2345 = DIRECTION ( 'NONE',  ( 0.000000000000000000, 0.000000000000000000, -1.000000000000000000 ) ) ;
#2346 = ORIENTED_EDGE ( 'NONE', *, *, #7434, .T. ) ;
#2347 = CARTESIAN_POINT ( 'NONE',  ( 4.573385150445044900, -19.31989681812820692, 6.000000000000000000 ) ) ;
#2348 = CONICAL_SURFACE ( 'NONE', #8283, 10.49999999999999467, 0.7853981633974497223 ) ;
#2349 = ORIENTED_EDGE ( 'NONE', *, *, #811, .F. ) ;
#2350 = ORIENTED_EDGE ( 'NONE', *, *, #7668, .T. ) ;
#2351 = CARTESIAN_POINT ( 'NONE',  ( -88.81638362644000040, 63.99516924618178848, -147.9984795835769944 ) ) ;
#2352 = ORIENTED_EDGE ( 'NONE', *, *, #11585, .F. ) ;
#2353 = CARTESIAN_POINT ( 'NONE',  ( 3.641294513787672660, -1.921088562373076236, 1.947552941946255389 ) ) ;
#2354 = CIRCLE ( 'NONE', #4612, 1.500000000000001332 ) ;
#2355 = DIRECTION ( 'NONE',  ( -0.000000000000000000, -0.000000000000000000, -1.000000000000000000 ) ) ;
#2356 = FACE_OUTER_BOUND ( 'NONE', #8011, .T. ) ;
#2357 =( GEOMETRIC_REPRESENTATION_CONTEXT ( 3 ) GLOBAL_UNCERTAINTY_ASSIGNED_CONTEXT ( ( #9786 ) ) GLOBAL_UNIT_ASSIGNED_CONTEXT ( ( #5290, #6536, #5372 ) ) REPRESENTATION_CONTEXT ( 'NONE', 'WORKASPACE' ) );
#2358 = CARTESIAN_POINT ( 'NONE',  ( -13.41835358098578723, 11.99999970914576330, -11.73358795631400753 ) ) ;
#2359 = AXIS2_PLACEMENT_3D ( 'NONE', #12424, #1563, #2962 ) ;
#2360 = LINE ( 'NONE', #10655, #12731 ) ;
#2361 = VERTEX_POINT ( 'NONE', #1477 ) ;
#2362 = DIRECTION ( 'NONE',  ( 0.000000000000000000, 0.000000000000000000, -1.000000000000000000 ) ) ;
#2363 = DIRECTION ( 'NONE',  ( -0.000000000000000000, -0.000000000000000000, -1.000000000000000000 ) ) ;
#2364 = MECHANICAL_DESIGN_GEOMETRIC_PRESENTATION_REPRESENTATION (  '', ( #9545 ), #388 ) ;
#2365 = VERTEX_POINT ( 'NONE', #10934 ) ;
#2366 = VECTOR ( 'NONE', #4232, 1000.000000000000000 ) ;
#2367 = CARTESIAN_POINT ( 'NONE',  ( -3.745604523531179897, -3.546874999999923173, 1.135144126415479793 ) ) ;
#2368 = ORIENTED_EDGE ( 'NONE', *, *, #322, .T. ) ;
#2369 = AXIS2_PLACEMENT_3D ( 'NONE', #13576, #1768, #601 ) ;
#2370 = ADVANCED_FACE ( 'NONE', ( #9532 ), #3654, .T. ) ;
#2371 = CARTESIAN_POINT ( 'NONE',  ( -2.463482987169076210, -0.9443750000000532552, -3.003366100166337649 ) ) ;
#2372 = CARTESIAN_POINT ( 'NONE',  ( -0.5946215730125156140, -5.371277108568085268, 3.300960504506171400 ) ) ;
#2373 = AXIS2_PLACEMENT_3D ( 'NONE', #2761, #361, #7515 ) ;
#2374 = CARTESIAN_POINT ( 'NONE',  ( 21.98164641901421135, 12.59999970914575940, -8.183940086454237317 ) ) ;
#2375 = VECTOR ( 'NONE', #2567, 1000.000000000000114 ) ;
#2376 = LINE ( 'NONE', #46, #11606 ) ;
#2377 = PLANE ( 'NONE',  #5028 ) ;
#2378 = CIRCLE ( 'NONE', #12053, 2.514916625122320948 ) ;
#2379 = FACE_OUTER_BOUND ( 'NONE', #213, .T. ) ;
#2380 = FACE_OUTER_BOUND ( 'NONE', #7641, .T. ) ;
#2381 = ORIENTED_EDGE ( 'NONE', *, *, #137, .F. ) ;
#2382 = DIRECTION ( 'NONE',  ( -1.000000000000000000, -9.422394424380278809E-16, 0.000000000000000000 ) ) ;
#2383 = EDGE_CURVE ( 'NONE', #9574, #1401, #10980, .T. ) ;
#2384 = ORIENTED_EDGE ( 'NONE', *, *, #9675, .F. ) ;
#2385 = PRODUCT ( 'MAIN GRIPPER BODY ENCLOSURE', 'MAIN GRIPPER BODY ENCLOSURE', '', ( #3530 ) ) ;
#2386 = DIRECTION ( 'NONE',  ( 1.000000000000000000, -0.000000000000000000, -0.000000000000000000 ) ) ;
#2387 = CARTESIAN_POINT ( 'NONE',  ( -2.013335231365205313, -2.928749999999985310, -3.010762893885848168 ) ) ;
#2388 = VERTEX_POINT ( 'NONE', #8450 ) ;
#2389 = AXIS2_PLACEMENT_3D ( 'NONE', #12300, #2593, #3760 ) ;
#2390 = EDGE_LOOP ( 'NONE', ( #14213, #2461 ) ) ;
#2391 = ADVANCED_FACE ( 'NONE', ( #10703 ), #7387, .F. ) ;
#2392 = ORIENTED_EDGE ( 'NONE', *, *, #8193, .T. ) ;
#2393 = AXIS2_PLACEMENT_3D ( 'NONE', #14035, #4728, #2236 ) ;
#2394 = CARTESIAN_POINT ( 'NONE',  ( -3.140138096963257297, -4.592963562373083342, 2.096990760703472567 ) ) ;
#2395 = DIRECTION ( 'NONE',  ( -1.000000000000000000, 0.000000000000000000, 0.000000000000000000 ) ) ;
#2396 = CYLINDRICAL_SURFACE ( 'NONE', #3642, 1.785937500000001066 ) ;
#2397 = DIRECTION ( 'NONE',  ( 0.000000000000000000, 0.000000000000000000, -1.000000000000000000 ) ) ;
#2398 = DIRECTION ( 'NONE',  ( 0.08715574274766155205, 6.505213034913022660E-16, -0.9961946980917452121 ) ) ;
#2399 = DIRECTION ( 'NONE',  ( 0.000000000000000000, -2.891205793294679017E-15, -1.000000000000000000 ) ) ;
#2400 = CIRCLE ( 'NONE', #11083, 1.199999999999710854 ) ;
#2401 = CARTESIAN_POINT ( 'NONE',  ( -46.58670980944423690, 0.000000000000000000, 89.50956111919107627 ) ) ;
#2402 = CARTESIAN_POINT ( 'NONE',  ( -2.874539946219666575, -4.178749999999989306, 1.919644203647528302 ) ) ;
#2403 = DIRECTION ( 'NONE',  ( -0.000000000000000000, -0.000000000000000000, -1.000000000000000000 ) ) ;
#2404 = VECTOR ( 'NONE', #12479, 1000.000000000000000 ) ;
#2405 = ORIENTED_EDGE ( 'NONE', *, *, #4909, .T. ) ;
#2406 = CYLINDRICAL_SURFACE ( 'NONE', #7294, 1.000000000000000888 ) ;
#2407 = EDGE_CURVE ( 'NONE', #2251, #8280, #5544, .T. ) ;
#2408 = ORIENTED_EDGE ( 'NONE', *, *, #598, .T. ) ;
#2409 = VERTEX_POINT ( 'NONE', #4970 ) ;
#2410 = ORIENTED_EDGE ( 'NONE', *, *, #13056, .T. ) ;
#2411 = EDGE_CURVE ( 'NONE', #4210, #1912, #14194, .T. ) ;
#2412 = DIRECTION ( 'NONE',  ( -0.08715574274766123286, 0.000000000000000000, 0.9961946980917453232 ) ) ;
#2413 = CARTESIAN_POINT ( 'NONE',  ( -3.586083906644841779, -3.069375000000151399, -0.3518610084925551384 ) ) ;
#2414 = VECTOR ( 'NONE', #8003, 1000.000000000000000 ) ;
#2415 = DIRECTION ( 'NONE',  ( 0.000000000000000000, 0.000000000000000000, 1.000000000000000000 ) ) ;
#2416 = LINE ( 'NONE', #9391, #12683 ) ;
#2417 = CARTESIAN_POINT ( 'NONE',  ( -1.770063184912698206, 2.057215485424382262, -4.499999999999998224 ) ) ;
#2418 = DIRECTION ( 'NONE',  ( 0.000000000000000000, -1.000000000000000000, 0.000000000000000000 ) ) ;
#2419 = EDGE_CURVE ( 'NONE', #10261, #13163, #6227, .T. ) ;
#2420 = CARTESIAN_POINT ( 'NONE',  ( 35.35543536254876074, -19.31989681812820692, 6.000000000000000000 ) ) ;
#2421 = CARTESIAN_POINT ( 'NONE',  ( -52.77438362643999881, 67.53201699523744139, -147.9984795835769944 ) ) ;
#2422 = DIRECTION ( 'NONE',  ( 0.000000000000000000, 1.000000000000000000, 0.000000000000000000 ) ) ;
#2423 = FACE_OUTER_BOUND ( 'NONE', #7051, .T. ) ;
#2424 = DIRECTION ( 'NONE',  ( 0.000000000000000000, -1.000000000000000000, 0.000000000000000000 ) ) ;
#2425 =( BOUNDED_CURVE ( )  B_SPLINE_CURVE ( 3, ( #9544, #10562, #11735, #5937 ),
 .UNSPECIFIED., .F., .T. ) 
 B_SPLINE_CURVE_WITH_KNOTS ( ( 4, 4 ),
 ( 3.141592653589792672, 4.712388980384706549 ),
 .UNSPECIFIED. ) 
 CURVE ( )  GEOMETRIC_REPRESENTATION_ITEM ( )  RATIONAL_B_SPLINE_CURVE ( ( 1.000000000000000000, 0.8047378541243609407, 0.8047378541243609407, 1.000000000000000000 ) ) 
 REPRESENTATION_ITEM ( '' )  );
#2426 = ORIENTED_EDGE ( 'NONE', *, *, #5920, .T. ) ;
#2427 = FACE_OUTER_BOUND ( 'NONE', #5067, .T. ) ;
#2428 = EDGE_CURVE ( 'NONE', #12810, #14328, #5808, .T. ) ;
#2429 = ORIENTED_EDGE ( 'NONE', *, *, #13010, .T. ) ;
#2430 = AXIS2_PLACEMENT_3D ( 'NONE', #13119, #1395, #2399 ) ;
#2431 = ORIENTED_EDGE ( 'NONE', *, *, #11974, .F. ) ;
#2432 = EDGE_CURVE ( 'NONE', #8073, #14575, #8306, .T. ) ;
#2433 = CARTESIAN_POINT ( 'NONE',  ( 2.767528002676985288, -0.1406250000000294209, -3.374716907253854092 ) ) ;
#2434 = ADVANCED_FACE ( 'NONE', ( #1237 ), #10625, .T. ) ;
#2435 = ORIENTED_EDGE ( 'NONE', *, *, #12919, .F. ) ;
#2436 = CARTESIAN_POINT ( 'NONE',  ( -3.223041131337215592, -1.608588562373021835, 2.647033509805598150 ) ) ;
#2437 = DIRECTION ( 'NONE',  ( -0.000000000000000000, 1.000000000000000000, -0.000000000000000000 ) ) ;
#2438 = DIRECTION ( 'NONE',  ( -1.000000000000000000, 0.000000000000000000, 0.000000000000000000 ) ) ;
#2439 = CARTESIAN_POINT ( 'NONE',  ( 4.785585838562195882, 2.054436331234747115, -0.7111221836281572672 ) ) ;
#2440 = CARTESIAN_POINT ( 'NONE',  ( -15.50000000000000000, -0.2038245569916614930, -23.94337567297399971 ) ) ;
#2441 = EDGE_LOOP ( 'NONE', ( #13075, #1953, #7685 ) ) ;
#2442 = CARTESIAN_POINT ( 'NONE',  ( -3.637955631634631981, -5.500000000000017764, 0.000000000000000000 ) ) ;
#2443 = DIRECTION ( 'NONE',  ( 0.000000000000000000, 0.000000000000000000, 1.000000000000000000 ) ) ;
#2444 = ORIENTED_EDGE ( 'NONE', *, *, #4016, .F. ) ;
#2445 = CIRCLE ( 'NONE', #14822, 1.999999999999989564 ) ;
#2446 = CARTESIAN_POINT ( 'NONE',  ( 2.736090332400194836, -3.875000000000003553, 2.737522629006357455 ) ) ;
#2447 = ORIENTED_EDGE ( 'NONE', *, *, #13031, .F. ) ;
#2448 = CARTESIAN_POINT ( 'NONE',  ( 2.481497852716095132, -0.7256250000000298295, -3.025965195089417747 ) ) ;
#2449 = CARTESIAN_POINT ( 'NONE',  ( 1.430388965971081561, -5.414568188701776030, 2.971966112566031715 ) ) ;
#2450 = DIRECTION ( 'NONE',  ( -1.287488025362404182E-15, -1.000000000000000000, 0.000000000000000000 ) ) ;
#2451 = DIRECTION ( 'NONE',  ( 0.000000000000000000, 0.000000000000000000, 1.000000000000000000 ) ) ;
#2452 = CYLINDRICAL_SURFACE ( 'NONE', #14580, 16.00000000000000000 ) ;
#2453 = FACE_OUTER_BOUND ( 'NONE', #5115, .T. ) ;
#2454 = CARTESIAN_POINT ( 'NONE',  ( -15.50000000000000000, -0.4000000000005236034, -19.20000000000052509 ) ) ;
#2455 = VERTEX_POINT ( 'NONE', #493 ) ;
#2456 = CYLINDRICAL_SURFACE ( 'NONE', #8274, 2.500000000000002220 ) ;
#2457 =( NAMED_UNIT ( * ) PLANE_ANGLE_UNIT ( ) SI_UNIT ( $, .RADIAN. ) );
#2458 = ORIENTED_EDGE ( 'NONE', *, *, #2913, .F. ) ;
#2459 = CARTESIAN_POINT ( 'NONE',  ( -84.27438362644100778, 99.17411849586700612, -182.2484795835770228 ) ) ;
#2460 = CARTESIAN_POINT ( 'NONE',  ( -2.533829858540610047, -3.209999999999945786, 2.535703909530143463 ) ) ;
#2461 = ORIENTED_EDGE ( 'NONE', *, *, #6878, .T. ) ;
#2462 = ORIENTED_EDGE ( 'NONE', *, *, #1726, .T. ) ;
#2463 = EDGE_LOOP ( 'NONE', ( #4360, #3971, #246, #11952 ) ) ;
#2464 = DIRECTION ( 'NONE',  ( 1.000000000000000000, 0.000000000000000000, 0.000000000000000000 ) ) ;
#2465 = CARTESIAN_POINT ( 'NONE',  ( 4.573385150445044900, -19.31989681812820692, 0.000000000000000000 ) ) ;
#2466 = ADVANCED_FACE ( 'NONE', ( #13049 ), #2406, .T. ) ;
#2467 = DIRECTION ( 'NONE',  ( 0.08715574274766160756, -6.299629708773494780E-18, -0.9961946980917452121 ) ) ;
#2468 = APPLICATION_CONTEXT ( 'automotive_design' ) ;
#2469 = DIRECTION ( 'NONE',  ( 0.000000000000000000, 0.000000000000000000, -1.000000000000000000 ) ) ;
#2470 = DIRECTION ( 'NONE',  ( -0.4999999999999832356, 0.000000000000000000, 0.8660254037844483666 ) ) ;
#2471 = PLANE ( 'NONE',  #9798 ) ;
#2472 = ADVANCED_FACE ( 'NONE', ( #3017, #6378 ), #2867, .T. ) ;
#2473 = CARTESIAN_POINT ( 'NONE',  ( -1.318845896519720284, -4.272500000000155396, 3.181678407182404023 ) ) ;
#2474 = FACE_OUTER_BOUND ( 'NONE', #10176, .T. ) ;
#2475 = ORIENTED_EDGE ( 'NONE', *, *, #5085, .T. ) ;
#2476 = B_SPLINE_CURVE_WITH_KNOTS ( 'NONE', 3,
 ( #14449, #11981, #3604, #1264, #8561, #3681 ),
 .UNSPECIFIED., .F., .F.,
 ( 4, 2, 4 ),
 ( 0.0002380763768129734448, 0.7291065797294591366, 1.457975083082105439 ),
 .UNSPECIFIED. ) ;
#2477 = DIRECTION ( 'NONE',  ( 0.000000000000000000, 1.000000000000000000, 0.000000000000000000 ) ) ;
#2478 = ORIENTED_EDGE ( 'NONE', *, *, #1366, .F. ) ;
#2479 = ORIENTED_EDGE ( 'NONE', *, *, #2304, .T. ) ;
#2480 = ORIENTED_EDGE ( 'NONE', *, *, #4140, .T. ) ;
#2481 = PLANE ( 'NONE',  #13926 ) ;
#2482 = DIRECTION ( 'NONE',  ( -0.000000000000000000, -0.000000000000000000, 1.000000000000000000 ) ) ;
#2483 = EDGE_CURVE ( 'NONE', #2967, #12409, #9991, .T. ) ;
#2484 = DIRECTION ( 'NONE',  ( 0.000000000000000000, 0.000000000000000000, -1.000000000000000000 ) ) ;
#2485 = DIRECTION ( 'NONE',  ( 1.000000000000000000, 0.000000000000000000, 0.000000000000000000 ) ) ;
#2486 = EDGE_CURVE ( 'NONE', #4841, #686, #9842, .T. ) ;
#2487 = CYLINDRICAL_SURFACE ( 'NONE', #8585, 3.499999999999999556 ) ;
#2488 = DIRECTION ( 'NONE',  ( -0.8660254037844482555, 0.000000000000000000, 0.4999999999999831801 ) ) ;
#2489 = DIRECTION ( 'NONE',  ( 0.000000000000000000, 1.000000000000000000, 0.000000000000000000 ) ) ;
#2490 = DIRECTION ( 'NONE',  ( 0.000000000000000000, 0.000000000000000000, 1.000000000000000000 ) ) ;
#2491 = DIRECTION ( 'NONE',  ( -0.000000000000000000, -0.000000000000000000, 1.000000000000000000 ) ) ;
#2492 = CARTESIAN_POINT ( 'NONE',  ( 17.18164641901421419, 11.99999970914575975, 0.8664120436859877872 ) ) ;
#2493 = ORIENTED_EDGE ( 'NONE', *, *, #6418, .F. ) ;
#2494 = CARTESIAN_POINT ( 'NONE',  ( 16.12213235744115636, -12.00000029085424202, 0.3029999373072352897 ) ) ;
#2495 = ORIENTED_EDGE ( 'NONE', *, *, #13972, .T. ) ;
#2496 = VECTOR ( 'NONE', #1895, 1000.000000000000000 ) ;
#2497 = ORIENTED_EDGE ( 'NONE', *, *, #4111, .T. ) ;
#2498 = FACE_OUTER_BOUND ( 'NONE', #8881, .T. ) ;
#2499 = EDGE_CURVE ( 'NONE', #13840, #8420, #3070, .T. ) ;
#2500 = CARTESIAN_POINT ( 'NONE',  ( 0.4250114624652890916, -0.2343749999999928668, -4.331188314191872557 ) ) ;
#2501 = VERTEX_POINT ( 'NONE', #13502 ) ;
#2502 = CARTESIAN_POINT ( 'NONE',  ( -2.312421387223750902, -1.655463562372999187, 3.463495667214802953 ) ) ;
#2503 = CONICAL_SURFACE ( 'NONE', #12164, 3.968749999999992895, 0.7155849933176756661 ) ;
#2504 = LINE ( 'NONE', #12065, #4501 ) ;
#2505 = EDGE_CURVE ( 'NONE', #382, #14751, #581, .T. ) ;
#2506 = PLANE ( 'NONE',  #881 ) ;
#2507 = AXIS2_PLACEMENT_3D ( 'NONE', #7567, #10094, #3977 ) ;
#2508 = CARTESIAN_POINT ( 'NONE',  ( 21.98164641901421135, -11.40000029085424238, 0.2664120436859911956 ) ) ;
#2509 = EDGE_CURVE ( 'NONE', #14684, #1190, #11094, .T. ) ;
#2510 = PRODUCT_DEFINITION_SHAPE ( 'NONE', 'NONE',  #15336 ) ;
#2511 = DIRECTION ( 'NONE',  ( -0.000000000000000000, 1.000000000000000000, -0.000000000000000000 ) ) ;
#2512 = EDGE_CURVE ( 'NONE', #6403, #10071, #4109, .T. ) ;
#2513 = ORIENTED_EDGE ( 'NONE', *, *, #615, .F. ) ;
#2514 = DIRECTION ( 'NONE',  ( 0.000000000000000000, 0.000000000000000000, -1.000000000000000000 ) ) ;
#2515 = DIRECTION ( 'NONE',  ( 0.8660254037844482555, 0.000000000000000000, 0.4999999999999831801 ) ) ;
#2516 = PRODUCT_CONTEXT ( 'NONE', #4069, 'mechanical' ) ;
#2517 = EDGE_LOOP ( 'NONE', ( #10301, #2950, #8307, #8615, #2732 ) ) ;
#2518 = DIRECTION ( 'NONE',  ( -1.000000000000000000, 0.000000000000000000, 0.000000000000000000 ) ) ;
#2519 = EDGE_CURVE ( 'NONE', #7520, #3938, #12234, .T. ) ;
#2520 = CARTESIAN_POINT ( 'NONE',  ( 0.7330380326264336333, -4.781250000000259348, 3.678172007241774732 ) ) ;
#2521 = ORIENTED_EDGE ( 'NONE', *, *, #14653, .T. ) ;
#2522 = AXIS2_PLACEMENT_3D ( 'NONE', #5733, #10674, #8044 ) ;
#2523 = CARTESIAN_POINT ( 'NONE',  ( 3.756292859848789689, -0.6318749999998841682, -1.140955529460117690 ) ) ;
#2524 = ADVANCED_FACE ( 'NONE', ( #13649 ), #14644, .F. ) ;
#2525 = DIRECTION ( 'NONE',  ( 0.000000000000000000, 1.000000000000000000, 0.000000000000000000 ) ) ;
#2526 = CIRCLE ( 'NONE', #2773, 2.320576762250993852 ) ;
#2527 = DIRECTION ( 'NONE',  ( -1.000000000000000000, 0.000000000000000000, 0.000000000000000000 ) ) ;
#2528 =( GEOMETRIC_REPRESENTATION_CONTEXT ( 3 ) GLOBAL_UNCERTAINTY_ASSIGNED_CONTEXT ( ( #936 ) ) GLOBAL_UNIT_ASSIGNED_CONTEXT ( ( #9896, #6439, #1754 ) ) REPRESENTATION_CONTEXT ( 'NONE', 'WORKASPACE' ) );
#2529 = CARTESIAN_POINT ( 'NONE',  ( 5.196152422706631135, 0.1227504548087541975, -1.122964458370237425E-15 ) ) ;
#2530 = CARTESIAN_POINT ( 'NONE',  ( 2.188996733326721955, -5.387487143035719406, 2.513283957937794355 ) ) ;
#2531 = DIRECTION ( 'NONE',  ( 0.000000000000000000, 1.000000000000000000, 0.000000000000000000 ) ) ;
#2532 = FACE_BOUND ( 'NONE', #13254, .T. ) ;
#2533 = AXIS2_PLACEMENT_3D ( 'NONE', #15204, #3585, #14204 ) ;
#2534 = EDGE_LOOP ( 'NONE', ( #2349, #8405, #14864, #11949 ) ) ;
#2535 = CARTESIAN_POINT ( 'NONE',  ( -52.77438362644100067, 99.17411849586700612, -182.2484795835770228 ) ) ;
#2536 = DIRECTION ( 'NONE',  ( 0.000000000000000000, 0.000000000000000000, 1.000000000000000000 ) ) ;
#2537 = ORIENTED_EDGE ( 'NONE', *, *, #8355, .F. ) ;
#2538 = PRESENTATION_LAYER_ASSIGNMENT (  '', '', ( #796 ) ) ;
#2539 = CYLINDRICAL_SURFACE ( 'NONE', #7797, 4.499999999999997335 ) ;
#2540 = CARTESIAN_POINT ( 'NONE',  ( 0.3508518002069098141, -3.350624999999907150, 3.548798009676431331 ) ) ;
#2541 = ORIENTED_EDGE ( 'NONE', *, *, #4236, .F. ) ;
#2542 = ORIENTED_EDGE ( 'NONE', *, *, #8874, .F. ) ;
#2543 = ORIENTED_EDGE ( 'NONE', *, *, #6202, .T. ) ;
#2544 = VECTOR ( 'NONE', #13814, 999.9999999999998863 ) ;
#2545 = CARTESIAN_POINT ( 'NONE',  ( -44.58670980944423690, 5.000000000000000000, 137.5095611191910621 ) ) ;
#2546 = CARTESIAN_POINT ( 'NONE',  ( -77.52077156573416516, 59.67411849586701322, -79.59847958357700293 ) ) ;
#2547 = CARTESIAN_POINT ( 'NONE',  ( -75.01311196519617397, 67.29799558322736175, -83.44847958357698303 ) ) ;
#2548 = AXIS2_PLACEMENT_3D ( 'NONE', #1748, #8655, #6498 ) ;
#2549 = LINE ( 'NONE', #7298, #13097 ) ;
#2550 = DIRECTION ( 'NONE',  ( 0.000000000000000000, 1.000000000000000000, 0.000000000000000000 ) ) ;
#2551 = CARTESIAN_POINT ( 'NONE',  ( -79.11147769456633227, 68.38713492810558137, -81.84847958357697451 ) ) ;
#2552 = CARTESIAN_POINT ( 'NONE',  ( -1.914696782014857490, -4.241249999999832987, 2.867854448260447775 ) ) ;
#2553 = DIRECTION ( 'NONE',  ( 0.000000000000000000, 0.000000000000000000, 1.000000000000000000 ) ) ;
#2554 = ORIENTED_EDGE ( 'NONE', *, *, #4854, .T. ) ;
#2555 = CIRCLE ( 'NONE', #2804, 16.50000000000000000 ) ;
#2556 = VECTOR ( 'NONE', #3416, 1000.000000000000114 ) ;
#2557 = ORIENTED_EDGE ( 'NONE', *, *, #9893, .F. ) ;
#2558 = EDGE_LOOP ( 'NONE', ( #11468, #1985 ) ) ;
#2559 = ORIENTED_EDGE ( 'NONE', *, *, #12932, .F. ) ;
#2560 = VERTEX_POINT ( 'NONE', #1851 ) ;
#2561 = VECTOR ( 'NONE', #9529, 1000.000000000000114 ) ;
#2562 = ADVANCED_FACE ( 'NONE', ( #7614 ), #14574, .F. ) ;
#2563 = DIRECTION ( 'NONE',  ( 2.551930889570660354E-15, -1.000000000000000000, 0.000000000000000000 ) ) ;
#2564 = CARTESIAN_POINT ( 'NONE',  ( -0.7342670381812395064, -4.718750000000252243, 3.686397723581088304 ) ) ;
#2565 = CARTESIAN_POINT ( 'NONE',  ( 16.99691247867024657, -3.779330867977714892, 1.266532794505838000 ) ) ;
#2566 = VECTOR ( 'NONE', #15021, 1000.000000000000000 ) ;
#2567 = DIRECTION ( 'NONE',  ( 0.08715574274766155205, 6.505213034913022660E-16, -0.9961946980917452121 ) ) ;
#2568 = DIRECTION ( 'NONE',  ( 0.000000000000000000, 0.000000000000000000, -1.000000000000000000 ) ) ;
#2569 = DIRECTION ( 'NONE',  ( -0.08715574274766176022, -4.320305823558445788E-16, 0.9961946980917453232 ) ) ;
#2570 = CARTESIAN_POINT ( 'NONE',  ( -69.77438362644001302, 82.17411849586700612, -79.49847958357700861 ) ) ;
#2571 = DIRECTION ( 'NONE',  ( 0.000000000000000000, 0.000000000000000000, -1.000000000000000000 ) ) ;
#2572 = CYLINDRICAL_SURFACE ( 'NONE', #12702, 3.499999999999999556 ) ;
#2573 = ORIENTED_EDGE ( 'NONE', *, *, #12019, .F. ) ;
#2574 = CARTESIAN_POINT ( 'NONE',  ( 16.21557691923156597, -12.00000029085576969, 0.2777084275547281322 ) ) ;
#2575 = ORIENTED_EDGE ( 'NONE', *, *, #764, .F. ) ;
#2576 = EDGE_LOOP ( 'NONE', ( #2479, #7271 ) ) ;
#2577 = ORIENTED_EDGE ( 'NONE', *, *, #982, .F. ) ;
#2578 = CARTESIAN_POINT ( 'NONE',  ( -35.58670980944424400, 0.000000000000000000, 131.2954986191910791 ) ) ;
#2579 = AXIS2_PLACEMENT_3D ( 'NONE', #11019, #391, #6458 ) ;
#2580 = EDGE_CURVE ( 'NONE', #6830, #7739, #8711, .T. ) ;
#2581 = AXIS2_PLACEMENT_3D ( 'NONE', #9752, #7529, #375 ) ;
#2582 = CARTESIAN_POINT ( 'NONE',  ( -2.047045606697944109, -0.3281249999999383271, -3.826439644639493487 ) ) ;
#2583 = CARTESIAN_POINT ( 'NONE',  ( -3.327015569456945876, -0.6085885623731795979, 2.728925429665365776 ) ) ;
#2584 = EDGE_CURVE ( 'NONE', #14784, #9846, #13962, .T. ) ;
#2585 = DIRECTION ( 'NONE',  ( 0.000000000000000000, 0.000000000000000000, -1.000000000000000000 ) ) ;
#2586 = DIRECTION ( 'NONE',  ( -1.000000000000000000, 0.000000000000000000, 0.000000000000000000 ) ) ;
#2587 = DIRECTION ( 'NONE',  ( -0.000000000000000000, -0.000000000000000000, 1.000000000000000000 ) ) ;
#2588 = DIRECTION ( 'NONE',  ( 9.422394424380278809E-16, -1.000000000000000000, 0.000000000000000000 ) ) ;
#2589 = CIRCLE ( 'NONE', #8536, 9.999999999999994671 ) ;
#2590 = CONICAL_SURFACE ( 'NONE', #4333, 3.968749999999992895, 0.7155849933176756661 ) ;
#2591 = DIRECTION ( 'NONE',  ( 0.000000000000000000, -1.000000000000000000, 0.000000000000000000 ) ) ;
#2592 = ORIENTED_EDGE ( 'NONE', *, *, #12952, .T. ) ;
#2593 = DIRECTION ( 'NONE',  ( 0.000000000000000000, 1.000000000000000000, 0.000000000000000000 ) ) ;
#2594 = ADVANCED_FACE ( 'NONE', ( #383 ), #8836, .T. ) ;
#2595 = ORIENTED_EDGE ( 'NONE', *, *, #4854, .F. ) ;
#2596 = CARTESIAN_POINT ( 'NONE',  ( 35.35543536254876074, -19.31989681812820692, 0.000000000000000000 ) ) ;
#2597 = CARTESIAN_POINT ( 'NONE',  ( -1.460276376564476175, -4.312500000000168754, -3.521769549316223102 ) ) ;
#2598 = ORIENTED_EDGE ( 'NONE', *, *, #12571, .F. ) ;
#2599 = VECTOR ( 'NONE', #7816, 1000.000000000000114 ) ;
#2600 = EDGE_CURVE ( 'NONE', #541, #11427, #6524, .T. ) ;
#2601 = AXIS2_PLACEMENT_3D ( 'NONE', #9462, #14201, #3582 ) ;
#2602 = ADVANCED_FACE ( 'NONE', ( #605 ), #5358, .T. ) ;
#2603 = CIRCLE ( 'NONE', #4348, 4.000000000000004441 ) ;
#2604 = CARTESIAN_POINT ( 'NONE',  ( -3.844997831300932756, -1.100624999999974429, 0.3801187285354425405 ) ) ;
#2605 = CARTESIAN_POINT ( 'NONE',  ( -1.165664718218115015, -5.359101102505690051, 3.151588464108890264 ) ) ;
#2606 = DIRECTION ( 'NONE',  ( -0.000000000000000000, -0.000000000000000000, 1.000000000000000000 ) ) ;
#2607 = EDGE_CURVE ( 'NONE', #9386, #8682, #10293, .T. ) ;
#2608 = CYLINDRICAL_SURFACE ( 'NONE', #4435, 3.499999999999999556 ) ;
#2609 = CARTESIAN_POINT ( 'NONE',  ( 0.000000000000000000, 5.000000000000000000, 0.000000000000000000 ) ) ;
#2610 = CARTESIAN_POINT ( 'NONE',  ( 15.50000000000000000, -0.2000000000000000111, -22.50000000000000000 ) ) ;
#2611 =( GEOMETRIC_REPRESENTATION_CONTEXT ( 3 ) GLOBAL_UNCERTAINTY_ASSIGNED_CONTEXT ( ( #6552 ) ) GLOBAL_UNIT_ASSIGNED_CONTEXT ( ( #10749, #10661, #9727 ) ) REPRESENTATION_CONTEXT ( 'NONE', 'WORKASPACE' ) );
#2612 = CARTESIAN_POINT ( 'NONE',  ( -15.50000000000000000, -0.2000000000000000111, 22.50000000000000000 ) ) ;
#2613 = CLOSED_SHELL ( 'NONE', ( #12366, #7367, #2056, #6299, #7918, #10068, #2915, #8105, #5476, #8957, #8780, #4692, #12623, #7735, #12757, #6698, #1675, #5462, #7135, #10168, #532, #12253, #899, #10008, #6937, #14155, #14929, #3162, #4325, #1381, #5487, #14829, #14357, #8586, #1446, #8672, #12538, #13439, #10430, #3236, #5236, #2370, #456 ) ) ;
#2614 = FACE_BOUND ( 'NONE', #11454, .T. ) ;
#2615 = CONICAL_SURFACE ( 'NONE', #376, 4.500000000000000888, 0.7853981633974500554 ) ;
#2616 = VERTEX_POINT ( 'NONE', #11546 ) ;
#2617 = AXIS2_PLACEMENT_3D ( 'NONE', #2863, #7610, #1698 ) ;
#2618 = DIRECTION ( 'NONE',  ( 0.000000000000000000, -0.1666666666666656582, -0.9860132971832695770 ) ) ;
#2619 = EDGE_CURVE ( 'NONE', #10610, #4759, #12726, .T. ) ;
#2620 = ORIENTED_EDGE ( 'NONE', *, *, #10107, .F. ) ;
#2621 = DIRECTION ( 'NONE',  ( 0.000000000000000000, 0.000000000000000000, 1.000000000000000000 ) ) ;
#2622 = CARTESIAN_POINT ( 'NONE',  ( -1.685726645313963656, -3.256874999999974651, 3.156579729352138930 ) ) ;
#2623 = ORIENTED_EDGE ( 'NONE', *, *, #6779, .F. ) ;
#2624 = VERTEX_POINT ( 'NONE', #1995 ) ;
#2625 = EDGE_CURVE ( 'NONE', #7520, #10300, #10368, .T. ) ;
#2626 = VERTEX_POINT ( 'NONE', #3470 ) ;
#2627 = EDGE_CURVE ( 'NONE', #2455, #2744, #14205, .T. ) ;
#2628 = AXIS2_PLACEMENT_3D ( 'NONE', #2596, #5239, #7659 ) ;
#2629 = CARTESIAN_POINT ( 'NONE',  ( -82.27438362643999881, 99.17411849586700612, -86.49847958357699440 ) ) ;
#2630 = VECTOR ( 'NONE', #4851, 1000.000000000000000 ) ;
#2631 = CIRCLE ( 'NONE', #12783, 2.042000000000002036 ) ;
#2632 = CARTESIAN_POINT ( 'NONE',  ( -1.266185496994490789, -5.191497722025411932, -3.348809276478283081 ) ) ;
#2633 = LINE ( 'NONE', #8441, #14219 ) ;
#2634 = CARTESIAN_POINT ( 'NONE',  ( -85.77438362644001302, 82.17411849586700612, -117.9984795835769944 ) ) ;
#2635 = DIRECTION ( 'NONE',  ( 0.000000000000000000, 0.000000000000000000, -1.000000000000000000 ) ) ;
#2636 = DIRECTION ( 'NONE',  ( 1.287488025362404182E-15, 1.000000000000000000, 0.000000000000000000 ) ) ;
#2637 = CARTESIAN_POINT ( 'NONE',  ( -57.02438362644099357, 99.17411849586700612, -182.2484795835770228 ) ) ;
#2638 = ORIENTED_EDGE ( 'NONE', *, *, #3185, .F. ) ;
#2639 = CARTESIAN_POINT ( 'NONE',  ( -52.77438362643999881, 65.17411849586700612, -145.2984795835770058 ) ) ;
#2640 = VERTEX_POINT ( 'NONE', #13801 ) ;
#2641 = AXIS2_PLACEMENT_3D ( 'NONE', #15205, #12893, #3428 ) ;
#2642 = ORIENTED_EDGE ( 'NONE', *, *, #13031, .T. ) ;
#2643 = VERTEX_POINT ( 'NONE', #13868 ) ;
#2644 = VECTOR ( 'NONE', #2720, 1000.000000000000000 ) ;
#2645 = ORIENTED_EDGE ( 'NONE', *, *, #2783, .T. ) ;
#2646 = CARTESIAN_POINT ( 'NONE',  ( 30.00000000000000000, 0.000000000000000000, -27.00000000000000000 ) ) ;
#2647 = CARTESIAN_POINT ( 'NONE',  ( 1.363531154075378282, -3.397500000000037712, 3.288412936073061399 ) ) ;
#2648 = SURFACE_STYLE_USAGE ( .BOTH. , #9689 ) ;
#2649 = CARTESIAN_POINT ( 'NONE',  ( 0.7448305450414310913, -4.218749999999887201, -3.751694669322447329 ) ) ;
#2650 = DIRECTION ( 'NONE',  ( 0.000000000000000000, -0.000000000000000000, 1.000000000000000000 ) ) ;
#2651 = DIRECTION ( 'NONE',  ( -1.000000000000000000, 0.000000000000000000, 0.000000000000000000 ) ) ;
#2652 = AXIS2_PLACEMENT_3D ( 'NONE', #15036, #3250, #5375 ) ;
#2653 = DIRECTION ( 'NONE',  ( -0.000000000000000000, -0.000000000000000000, 1.000000000000000000 ) ) ;
#2654 = FACE_BOUND ( 'NONE', #7974, .T. ) ;
#2655 = CARTESIAN_POINT ( 'NONE',  ( -57.27438362644000591, 65.17411849586700612, -86.49847958357699440 ) ) ;
#2656 = DIRECTION ( 'NONE',  ( 0.000000000000000000, 1.000000000000000000, 0.000000000000000000 ) ) ;
#2657 = FACE_BOUND ( 'NONE', #4847, .T. ) ;
#2658 = VERTEX_POINT ( 'NONE', #910 ) ;
#2659 = DIRECTION ( 'NONE',  ( -2.551930889570659960E-15, 1.000000000000000000, 0.000000000000000000 ) ) ;
#2660 = ORIENTED_EDGE ( 'NONE', *, *, #13338, .F. ) ;
#2661 = B_SPLINE_CURVE_WITH_KNOTS ( 'NONE', 3,
 ( #12820, #10397, #6929, #13900, #12979, #13065, #6857, #11647, #4518, #11881, #5771, #2417, #9392, #9464 ),
 .UNSPECIFIED., .F., .F.,
 ( 4, 2, 2, 2, 2, 2, 4 ),
 ( 0.002714574482386751184, 0.003387943617500365975, 0.004061312752613980767, 0.005408051022841208616, 0.006081420157954823408, 0.006754789293068438200, 0.008101527563295666048 ),
 .UNSPECIFIED. ) ;
#2662 = ORIENTED_EDGE ( 'NONE', *, *, #11510, .T. ) ;
#2663 = CARTESIAN_POINT ( 'NONE',  ( -3.336666538900097123, -5.084999999999988418, 0.001247370357356067296 ) ) ;
#2664 = CIRCLE ( 'NONE', #8847, 2.750000000000002665 ) ;
#2665 = AXIS2_PLACEMENT_3D ( 'NONE', #12777, #11378, #10059 ) ;
#2666 = DIRECTION ( 'NONE',  ( -0.000000000000000000, 1.000000000000000000, 4.336808689942017736E-16 ) ) ;
#2667 = CARTESIAN_POINT ( 'NONE',  ( 0.001503091390574608048, -1.749213562373128195, 4.152102130272123937 ) ) ;
#2668 = LINE ( 'NONE', #2903, #7842 ) ;
#2669 = CYLINDRICAL_SURFACE ( 'NONE', #2016, 16.50000000000000000 ) ;
#2670 = DIRECTION ( 'NONE',  ( 0.000000000000000000, -4.130293990420970006E-17, 1.000000000000000000 ) ) ;
#2671 = CARTESIAN_POINT ( 'NONE',  ( -52.77438362644100067, 101.5320169952374414, -147.9984795835769944 ) ) ;
#2672 = EDGE_CURVE ( 'NONE', #12055, #2078, #11623, .T. ) ;
#2673 = AXIS2_PLACEMENT_3D ( 'NONE', #7166, #9543, #7237 ) ;
#2674 = PLANE ( 'NONE',  #10421 ) ;
#2675 = ORIENTED_EDGE ( 'NONE', *, *, #13598, .F. ) ;
#2676 = CARTESIAN_POINT ( 'NONE',  ( -44.58670980944423690, 5.000000000000000000, 137.5095611191910621 ) ) ;
#2677 = EDGE_CURVE ( 'NONE', #4603, #3159, #6063, .T. ) ;
#2678 = VERTEX_POINT ( 'NONE', #8048 ) ;
#2679 = CARTESIAN_POINT ( 'NONE',  ( -35.58670980944424400, 0.000000000000000000, 127.7236236191910734 ) ) ;
#2680 = CARTESIAN_POINT ( 'NONE',  ( 1.766265845880009788, -4.828125000000014211, 3.301533676270316686 ) ) ;
#2681 = ORIENTED_EDGE ( 'NONE', *, *, #14758, .F. ) ;
#2682 = CARTESIAN_POINT ( 'NONE',  ( -3.719851489431995173, -4.467963562373030051, -0.7385069234750470946 ) ) ;
#2683 = AXIS2_PLACEMENT_3D ( 'NONE', #15264, #9524, #7147 ) ;
#2684 = CARTESIAN_POINT ( 'NONE',  ( -2.976231983981160845, -1.194374999999927578, 2.444352914378567387 ) ) ;
#2685 = DIRECTION ( 'NONE',  ( 0.8660254037844381525, 1.060575238724905436E-16, -0.5000000000000007772 ) ) ;
#2686 = DIRECTION ( 'NONE',  ( -0.000000000000000000, -4.336808689942017736E-16, 1.000000000000000000 ) ) ;
#2687 = ADVANCED_FACE ( 'NONE', ( #12630 ), #3234, .T. ) ;
#2688 = DIRECTION ( 'NONE',  ( 0.000000000000000000, 0.000000000000000000, 1.000000000000000000 ) ) ;
#2689 = CARTESIAN_POINT ( 'NONE',  ( -86.77438362644100778, 99.17411849586700612, -147.9984795835769944 ) ) ;
#2690 = FACE_BOUND ( 'NONE', #2225, .T. ) ;
#2691 = DIRECTION ( 'NONE',  ( -0.000000000000000000, -0.000000000000000000, 1.000000000000000000 ) ) ;
#2692 = DIRECTION ( 'NONE',  ( 0.003614861529251474706, 0.000000000000000000, -0.9999934663667180423 ) ) ;
#2693 = EDGE_CURVE ( 'NONE', #9916, #15330, #9251, .T. ) ;
#2694 = LINE ( 'NONE', #14553, #12443 ) ;
#2695 = VERTEX_POINT ( 'NONE', #12866 ) ;
#2696 = ORIENTED_EDGE ( 'NONE', *, *, #8538, .T. ) ;
#2697 = ORIENTED_EDGE ( 'NONE', *, *, #1954, .F. ) ;
#2698 = EDGE_LOOP ( 'NONE', ( #11113, #11513, #935, #14785, #1040 ) ) ;
#2699 = CARTESIAN_POINT ( 'NONE',  ( 3.059130242547762002, -2.491250000000117204, 2.045191655759115434 ) ) ;
#2700 = ORIENTED_EDGE ( 'NONE', *, *, #1821, .T. ) ;
#2701 = ORIENTED_EDGE ( 'NONE', *, *, #13036, .F. ) ;
#2702 = ADVANCED_FACE ( 'NONE', ( #11385 ), #984, .F. ) ;
#2703 = EDGE_CURVE ( 'NONE', #13582, #8436, #10210, .T. ) ;
#2704 = DIRECTION ( 'NONE',  ( 0.000000000000000000, 0.000000000000000000, 1.000000000000000000 ) ) ;
#2705 = CARTESIAN_POINT ( 'NONE',  ( 2.400236239102856661, -5.117328313055176103, -2.785141875113248844 ) ) ;
#2706 = EDGE_CURVE ( 'NONE', #9489, #4222, #6970, .T. ) ;
#2707 = DIRECTION ( 'NONE',  ( 0.000000000000000000, -1.000000000000000000, 0.000000000000000000 ) ) ;
#2708 = CARTESIAN_POINT ( 'NONE',  ( 3.039268535905459423, -0.4995676945082513920, -2.698502599271650038 ) ) ;
#2709 = CARTESIAN_POINT ( 'NONE',  ( -15.50000000000000000, -0.2000000000000000111, 19.20000000000052509 ) ) ;
#2710 = EDGE_CURVE ( 'NONE', #8436, #14943, #3306, .T. ) ;
#2711 = CARTESIAN_POINT ( 'NONE',  ( 15.50000000000000000, -1.037157890325000054, 22.50000000000000000 ) ) ;
#2712 = ADVANCED_FACE ( 'NONE', ( #3168 ), #10439, .F. ) ;
#2713 = ORIENTED_EDGE ( 'NONE', *, *, #6884, .T. ) ;
#2714 = DIRECTION ( 'NONE',  ( 0.000000000000000000, 0.000000000000000000, -1.000000000000000000 ) ) ;
#2715 = ORIENTED_EDGE ( 'NONE', *, *, #13140, .T. ) ;
#2716 = ORIENTED_EDGE ( 'NONE', *, *, #1096, .T. ) ;
#2717 = ORIENTED_EDGE ( 'NONE', *, *, #4485, .F. ) ;
#2718 = ORIENTED_EDGE ( 'NONE', *, *, #13441, .F. ) ;
#2719 = CARTESIAN_POINT ( 'NONE',  ( 3.503842902704710216, -2.631874999999911147, -1.061889326425361268 ) ) ;
#2720 = DIRECTION ( 'NONE',  ( -1.287488025362404182E-15, -1.000000000000000000, 0.000000000000000000 ) ) ;
#2721 = CARTESIAN_POINT ( 'NONE',  ( -3.787710864223658991, -4.499999999999990230, 0.001388818612877307929 ) ) ;
#2722 = FACE_BOUND ( 'NONE', #7540, .T. ) ;
#2723 = EDGE_CURVE ( 'NONE', #3944, #4925, #8518, .T. ) ;
#2724 = CARTESIAN_POINT ( 'NONE',  ( -96.77438362643999881, 65.17411849586700612, -79.59847958357700293 ) ) ;
#2725 = LINE ( 'NONE', #12046, #4560 ) ;
#2726 = DIRECTION ( 'NONE',  ( 0.000000000000000000, 0.000000000000000000, -1.000000000000000000 ) ) ;
#2727 = DIRECTION ( 'NONE',  ( 0.000000000000000000, 1.000000000000000000, 0.000000000000000000 ) ) ;
#2728 = CARTESIAN_POINT ( 'NONE',  ( 16.75000000000000000, -0.2038245569916320166, -23.22168783648699986 ) ) ;
#2729 = ORIENTED_EDGE ( 'NONE', *, *, #15169, .T. ) ;
#2730 = CARTESIAN_POINT ( 'NONE',  ( -82.52438362643998460, 65.17411849586700612, -182.2484795835770228 ) ) ;
#2731 = EDGE_LOOP ( 'NONE', ( #8430, #13992, #7902, #2554 ) ) ;
#2732 = ORIENTED_EDGE ( 'NONE', *, *, #11605, .F. ) ;
#2733 = ORIENTED_EDGE ( 'NONE', *, *, #12834, .T. ) ;
#2734 = CARTESIAN_POINT ( 'NONE',  ( -3.199287326323787539, -5.038124999999881837, -0.9691876696830880045 ) ) ;
#2735 = CARTESIAN_POINT ( 'NONE',  ( -13.41835358098578723, 11.99999970914576863, -56.77834603255778489 ) ) ;
#2736 = CARTESIAN_POINT ( 'NONE',  ( -2.785343681203863664, -4.991249999999938680, -1.859602269982785883 ) ) ;
#2737 = DIRECTION ( 'NONE',  ( 0.000000000000000000, 0.000000000000000000, -1.000000000000000000 ) ) ;
#2738 = FACE_BOUND ( 'NONE', #10888, .T. ) ;
#2739 = CARTESIAN_POINT ( 'NONE',  ( -1.629699455448989389E-14, 8.699999999999999289, 5.655858585055787181E-29 ) ) ;
#2740 = DIRECTION ( 'NONE',  ( 0.000000000000000000, -1.000000000000000000, -0.000000000000000000 ) ) ;
#2741 = DIRECTION ( 'NONE',  ( 1.000000000000000000, 0.000000000000000000, 0.000000000000000000 ) ) ;
#2742 = ORIENTED_EDGE ( 'NONE', *, *, #9043, .F. ) ;
#2743 = FACE_OUTER_BOUND ( 'NONE', #12732, .T. ) ;
#2744 = VERTEX_POINT ( 'NONE', #4412 ) ;
#2745 = AXIS2_PLACEMENT_3D ( 'NONE', #41, #266, #7585 ) ;
#2746 =( NAMED_UNIT ( * ) PLANE_ANGLE_UNIT ( ) SI_UNIT ( $, .RADIAN. ) );
#2747 = CARTESIAN_POINT ( 'NONE',  ( 2.225207906715364281, -2.843749999999932943, 3.332158947996217702 ) ) ;
#2748 = VERTEX_POINT ( 'NONE', #12704 ) ;
#2749 = CARTESIAN_POINT ( 'NONE',  ( -2.691423129642354084, -4.374213562373147290, -2.689451441446156554 ) ) ;
#2750 = AXIS2_PLACEMENT_3D ( 'NONE', #13412, #3789, #4098 ) ;
#2751 = CYLINDRICAL_SURFACE ( 'NONE', #3501, 2.750000000000002665 ) ;
#2752 = EDGE_CURVE ( 'NONE', #8702, #12591, #329, .T. ) ;
#2753 = ADVANCED_BREP_SHAPE_REPRESENTATION ( '', ( #5610, #285 ), #8229 ) ;
#2754 = LINE ( 'NONE', #2993, #1618 ) ;
#2755 = CARTESIAN_POINT ( 'NONE',  ( -77.82438362644001018, 82.17411849586700612, -85.04847958357699156 ) ) ;
#2756 = CARTESIAN_POINT ( 'NONE',  ( -48.52438362644100067, 99.17411849586700612, -149.9984795835770228 ) ) ;
#2757 = AXIS2_PLACEMENT_3D ( 'NONE', #6945, #5788, #10496 ) ;
#2758 = CARTESIAN_POINT ( 'NONE',  ( -52.77438362644100067, 99.17411849586700612, -147.9984795835769944 ) ) ;
#2759 = DIRECTION ( 'NONE',  ( -1.000000000000000000, 0.000000000000000000, 0.000000000000000000 ) ) ;
#2760 = CARTESIAN_POINT ( 'NONE',  ( -4.522482571421202024, 10.99999970914572778, 70.03692566716178192 ) ) ;
#2761 = CARTESIAN_POINT ( 'NONE',  ( -86.77438362644100778, 99.17411849586700612, -150.4984795835770228 ) ) ;
#2762 = CARTESIAN_POINT ( 'NONE',  ( -91.02438362643999881, 65.17411849586700612, -149.9984795835770228 ) ) ;
#2763 = VECTOR ( 'NONE', #1798, 1000.000000000000000 ) ;
#2764 = VERTEX_POINT ( 'NONE', #9285 ) ;
#2765 = VERTEX_POINT ( 'NONE', #14023 ) ;
#2766 = CIRCLE ( 'NONE', #9702, 4.499999999999997335 ) ;
#2767 = ORIENTED_EDGE ( 'NONE', *, *, #11386, .T. ) ;
#2768 = APPLICATION_CONTEXT ( 'automotive_design' ) ;
#2769 = LINE ( 'NONE', #9975, #10766 ) ;
#2770 = CARTESIAN_POINT ( 'NONE',  ( -1.439523803302256599, -1.897500000000171383, -3.471712813344601578 ) ) ;
#2771 = ORIENTED_EDGE ( 'NONE', *, *, #7665, .F. ) ;
#2772 = EDGE_CURVE ( 'NONE', #4558, #134, #1824, .T. ) ;
#2773 = AXIS2_PLACEMENT_3D ( 'NONE', #12585, #12353, #1944 ) ;
#2774 = DIRECTION ( 'NONE',  ( 1.000000000000000000, 0.000000000000000000, 0.000000000000000000 ) ) ;
#2775 = CARTESIAN_POINT ( 'NONE',  ( -3.036530611102517874, -5.238391572205651769, -1.778739313110275999 ) ) ;
#2776 = VECTOR ( 'NONE', #10658, 1000.000000000000000 ) ;
#2777 = CARTESIAN_POINT ( 'NONE',  ( -59.02799568714584666, 0.000000000000000000, -79.59847958357700293 ) ) ;
#2778 = FACE_OUTER_BOUND ( 'NONE', #3285, .T. ) ;
#2779 = FACE_OUTER_BOUND ( 'NONE', #5317, .T. ) ;
#2780 = FACE_OUTER_BOUND ( 'NONE', #10018, .T. ) ;
#2781 = DIRECTION ( 'NONE',  ( 1.000000000000000000, 0.000000000000000000, 0.000000000000000000 ) ) ;
#2782 = CIRCLE ( 'NONE', #6761, 1.000000000000000888 ) ;
#2783 = EDGE_CURVE ( 'NONE', #11570, #11860, #8363, .T. ) ;
#2784 = VERTEX_POINT ( 'NONE', #11929 ) ;
#2785 = DIRECTION ( 'NONE',  ( 0.000000000000000000, 0.000000000000000000, 1.000000000000000000 ) ) ;
#2786 = ORIENTED_EDGE ( 'NONE', *, *, #10162, .T. ) ;
#2787 = ORIENTED_EDGE ( 'NONE', *, *, #8789, .F. ) ;
#2788 = EDGE_LOOP ( 'NONE', ( #7966, #6101, #4257, #9700, #13915 ) ) ;
#2789 = ORIENTED_EDGE ( 'NONE', *, *, #12238, .F. ) ;
#2790 = VECTOR ( 'NONE', #14472, 1000.000000000000000 ) ;
#2791 = EDGE_CURVE ( 'NONE', #7742, #5220, #3703, .T. ) ;
#2792 = ORIENTED_EDGE ( 'NONE', *, *, #11668, .T. ) ;
#2793 = DIRECTION ( 'NONE',  ( -0.08715574274766164919, 0.000000000000000000, 0.9961946980917453232 ) ) ;
#2794 = CARTESIAN_POINT ( 'NONE',  ( 1.096135970525389913, -1.788124999999989750, -3.610092524386871560 ) ) ;
#2795 = EDGE_CURVE ( 'NONE', #13765, #13261, #12010, .T. ) ;
#2796 = AXIS2_PLACEMENT_3D ( 'NONE', #3859, #12153, #7436 ) ;
#2797 =( NAMED_UNIT ( * ) PLANE_ANGLE_UNIT ( ) SI_UNIT ( $, .RADIAN. ) );
#2798 = CARTESIAN_POINT ( 'NONE',  ( 3.833377307806092649, -4.015625000000129674, -0.3765428855675501119 ) ) ;
#2799 = FACE_OUTER_BOUND ( 'NONE', #11571, .T. ) ;
#2800 = CARTESIAN_POINT ( 'NONE',  ( 16.75000000000000000, -0.2038245569916320166, 21.77831216351300014 ) ) ;
#2801 = CARTESIAN_POINT ( 'NONE',  ( -86.77438362644001302, 99.17411849586700612, -79.59847958357700293 ) ) ;
#2802 = CARTESIAN_POINT ( 'NONE',  ( -81.27438362643999881, 82.17411849586700612, -83.44847958357698303 ) ) ;
#2803 = DIRECTION ( 'NONE',  ( 9.035018104045788110E-17, -0.9860132971832695770, 0.1666666666666656027 ) ) ;
#2804 = AXIS2_PLACEMENT_3D ( 'NONE', #12999, #14081, #2277 ) ;
#2805 = DIRECTION ( 'NONE',  ( -1.000000000000000000, 0.000000000000000000, 0.000000000000000000 ) ) ;
#2806 = CIRCLE ( 'NONE', #8504, 2.750000000000002665 ) ;
#2807 = CARTESIAN_POINT ( 'NONE',  ( -69.09337542095276774, 89.17411849586704875, -44.02377680093037071 ) ) ;
#2808 = ADVANCED_FACE ( 'NONE', ( #6210 ), #1378, .T. ) ;
#2809 = ORIENTED_EDGE ( 'NONE', *, *, #3062, .T. ) ;
#2810 = CARTESIAN_POINT ( 'NONE',  ( -52.77438362644000591, 99.17411849586700612, -145.4984795835769660 ) ) ;
#2811 = ORIENTED_EDGE ( 'NONE', *, *, #11069, .F. ) ;
#2812 = CIRCLE ( 'NONE', #8007, 2.000000000000001776 ) ;
#2813 = ORIENTED_EDGE ( 'NONE', *, *, #5660, .F. ) ;
#2814 = ORIENTED_EDGE ( 'NONE', *, *, #10541, .T. ) ;
#2815 = UNCERTAINTY_MEASURE_WITH_UNIT (LENGTH_MEASURE( 1.000000000000000082E-05 ), #7825, 'distance_accuracy_value', 'NONE');
#2816 = CARTESIAN_POINT ( 'NONE',  ( 3.135427973343691832, -5.538124999999991971, 0.9519854854112211884 ) ) ;
#2817 = EDGE_CURVE ( 'NONE', #4608, #5722, #13107, .T. ) ;
#2818 = VECTOR ( 'NONE', #8960, 1000.000000000000000 ) ;
#2819 = CARTESIAN_POINT ( 'NONE',  ( -2.488972454571050985, -5.975625000000068354, -2.041081048424583155 ) ) ;
#2820 = CIRCLE ( 'NONE', #11487, 2.042000000000002036 ) ;
#2821 = DIRECTION ( 'NONE',  ( 0.08715574274766167695, 0.000000000000000000, -0.9961946980917453232 ) ) ;
#2822 = CARTESIAN_POINT ( 'NONE',  ( -69.77438362644001302, 81.46011849586699327, -81.84847958357697451 ) ) ;
#2823 = AXIS2_PLACEMENT_3D ( 'NONE', #7947, #6806, #887 ) ;
#2824 = PLANE ( 'NONE',  #12582 ) ;
#2825 = DIRECTION ( 'NONE',  ( -1.000000000000000000, 0.000000000000000000, -0.000000000000000000 ) ) ;
#2826 = FACE_OUTER_BOUND ( 'NONE', #6846, .T. ) ;
#2827 = EDGE_LOOP ( 'NONE', ( #2211, #4842, #5535, #10590 ) ) ;
#2828 = FACE_OUTER_BOUND ( 'NONE', #4434, .T. ) ;
#2829 = AXIS2_PLACEMENT_3D ( 'NONE', #10249, #12600, #7866 ) ;
#2830 = AXIS2_PLACEMENT_3D ( 'NONE', #4796, #3633, #12102 ) ;
#2831 = ORIENTED_EDGE ( 'NONE', *, *, #12760, .F. ) ;
#2832 =( NAMED_UNIT ( * ) SI_UNIT ( $, .STERADIAN. ) SOLID_ANGLE_UNIT ( ) );
#2833 = CARTESIAN_POINT ( 'NONE',  ( -2.264039642164870969, -2.343749999999985789, -3.385713959793517080 ) ) ;
#2834 = VERTEX_POINT ( 'NONE', #14325 ) ;
#2835 = AXIS2_PLACEMENT_3D ( 'NONE', #13711, #5422, #7675 ) ;
#2836 = DIRECTION ( 'NONE',  ( 1.000000000000000000, 0.000000000000000000, 0.000000000000000000 ) ) ;
#2837 = VECTOR ( 'NONE', #9687, 1000.000000000000000 ) ;
#2838 = AXIS2_PLACEMENT_3D ( 'NONE', #9242, #13980, #10250 ) ;
#2839 = DIRECTION ( 'NONE',  ( -1.000000000000000000, 0.000000000000000000, 0.000000000000000000 ) ) ;
#2840 = CARTESIAN_POINT ( 'NONE',  ( -6.714472293954755422, -12.00000029085427578, 37.72291661448763733 ) ) ;
#2841 = LINE ( 'NONE', #13905, #8539 ) ;
#2842 = CARTESIAN_POINT ( 'NONE',  ( -102.2743836264399988, 104.6741184958670061, -15.85886927678779834 ) ) ;
#2843 = CARTESIAN_POINT ( 'NONE',  ( -0.2250800284370903792, 2.375126721000841101, 4.500000000000000888 ) ) ;
#2844 = DIRECTION ( 'NONE',  ( -0.000000000000000000, 1.000000000000000000, -0.000000000000000000 ) ) ;
#2845 = CARTESIAN_POINT ( 'NONE',  ( -84.27438362644100778, 99.17411849586700612, -145.2984795835770058 ) ) ;
#2846 = LINE ( 'NONE', #5334, #38 ) ;
#2847 = VERTEX_POINT ( 'NONE', #14249 ) ;
#2848 = EDGE_CURVE ( 'NONE', #4755, #3140, #10765, .T. ) ;
#2849 = CIRCLE ( 'NONE', #861, 8.124999999999992895 ) ;
#2850 = EDGE_LOOP ( 'NONE', ( #1376, #839, #3022, #1061 ) ) ;
#2851 = DIRECTION ( 'NONE',  ( -0.08715574274766162144, 0.000000000000000000, 0.9961946980917453232 ) ) ;
#2852 = CARTESIAN_POINT ( 'NONE',  ( 3.783562653031028677, -1.569374999999871845, 0.3712484392075320883 ) ) ;
#2853 = ORIENTED_EDGE ( 'NONE', *, *, #10839, .F. ) ;
#2854 = AXIS2_PLACEMENT_3D ( 'NONE', #4129, #1494, #8696 ) ;
#2855 = CARTESIAN_POINT ( 'NONE',  ( -73.80978675135780520, 64.78624853950366003, -81.84847958357697451 ) ) ;
#2856 = PRODUCT_DEFINITION_SHAPE ( 'NONE', 'NONE',  #7626 ) ;
#2857 = PLANE ( 'NONE',  #6877 ) ;
#2858 = VECTOR ( 'NONE', #14855, 1000.000000000000000 ) ;
#2859 = DIRECTION ( 'NONE',  ( 0.000000000000000000, 0.000000000000000000, 1.000000000000000000 ) ) ;
#2860 = PRESENTATION_LAYER_ASSIGNMENT (  '', '', ( #11288 ) ) ;
#2861 = CARTESIAN_POINT ( 'NONE',  ( -3.121185083186896581, -0.4995676945082675457, -2.860075285120150301 ) ) ;
#2862 = AXIS2_PLACEMENT_3D ( 'NONE', #2454, #15163, #2298 ) ;
#2863 = CARTESIAN_POINT ( 'NONE',  ( -15.50000000000000000, -5.000000000000000000, 22.50000000000000000 ) ) ;
#2864 = EDGE_CURVE ( 'NONE', #8823, #7562, #2820, .T. ) ;
#2865 = DIRECTION ( 'NONE',  ( -0.8660254037844482555, 0.000000000000000000, -0.4999999999999831801 ) ) ;
#2866 = ORIENTED_EDGE ( 'NONE', *, *, #27, .F. ) ;
#2867 = PLANE ( 'NONE',  #13235 ) ;
#2868 = ADVANCED_FACE ( 'NONE', ( #13176 ), #2456, .T. ) ;
#2869 = ORIENTED_EDGE ( 'NONE', *, *, #8012, .T. ) ;
#2870 = EDGE_LOOP ( 'NONE', ( #14382, #8170, #1463, #2266, #1478, #6999, #9026, #15219 ) ) ;
#2871 = ORIENTED_EDGE ( 'NONE', *, *, #7538, .F. ) ;
#2872 = VECTOR ( 'NONE', #10035, 1000.000000000000114 ) ;
#2873 = ORIENTED_EDGE ( 'NONE', *, *, #7651, .F. ) ;
#2874 = ORIENTED_EDGE ( 'NONE', *, *, #6690, .T. ) ;
#2875 = AXIS2_PLACEMENT_3D ( 'NONE', #3754, #15225, #7186 ) ;
#2876 = CARTESIAN_POINT ( 'NONE',  ( -59.02799568714584666, 103.6741184958669919, -152.4984795835769944 ) ) ;
#2877 = CIRCLE ( 'NONE', #14262, 0.2000000000005261458 ) ;
#2878 = CARTESIAN_POINT ( 'NONE',  ( -3.579091221414520518, -2.038125000000108322, -1.084269867492441586 ) ) ;
#2879 = PLANE ( 'NONE',  #1118 ) ;
#2880 = CARTESIAN_POINT ( 'NONE',  ( 2.968551569176787197, -4.109374999999867661, -2.434929705433495073 ) ) ;
#2881 = PLANE ( 'NONE',  #10978 ) ;
#2882 = CARTESIAN_POINT ( 'NONE',  ( -9.503456061879925088, 11.99999970914574021, 69.60114695342350899 ) ) ;
#2883 = CARTESIAN_POINT ( 'NONE',  ( -52.77438362644100067, 99.17411849586700612, -147.9984795835769944 ) ) ;
#2884 = CARTESIAN_POINT ( 'NONE',  ( -0.4212280308283230523, -0.7343750000000048850, 4.265137983724988757 ) ) ;
#2885 = CIRCLE ( 'NONE', #5884, 0.2000000000005261458 ) ;
#2886 = DIRECTION ( 'NONE',  ( 0.5000000000000003331, 0.8660254037844384856, 0.000000000000000000 ) ) ;
#2887 = EDGE_CURVE ( 'NONE', #6165, #8182, #834, .T. ) ;
#2888 = CARTESIAN_POINT ( 'NONE',  ( -102.2743836264399988, 99.17411849586700612, -15.85886927678779834 ) ) ;
#2889 = CARTESIAN_POINT ( 'NONE',  ( -66.51083064278755330, 89.17411849586699191, -44.70344037800860804 ) ) ;
#2890 = ORIENTED_EDGE ( 'NONE', *, *, #3751, .T. ) ;
#2891 = CIRCLE ( 'NONE', #5629, 4.000000000000004441 ) ;
#2892 = CARTESIAN_POINT ( 'NONE',  ( 3.250000000000017764, 7.362500000000000711, 0.000000000000000000 ) ) ;
#2893 = ADVANCED_FACE ( 'NONE', ( #7207 ), #10916, .F. ) ;
#2894 = ORIENTED_EDGE ( 'NONE', *, *, #12670, .F. ) ;
#2895 = ORIENTED_EDGE ( 'NONE', *, *, #9965, .F. ) ;
#2896 = ORIENTED_EDGE ( 'NONE', *, *, #4184, .F. ) ;
#2897 = CARTESIAN_POINT ( 'NONE',  ( 2.729225460314726348, -5.491250000000120757, 1.824606648063346048 ) ) ;
#2898 = DIRECTION ( 'NONE',  ( 0.000000000000000000, 1.000000000000000000, 0.000000000000000000 ) ) ;
#2899 = VECTOR ( 'NONE', #13780, 1000.000000000000000 ) ;
#2900 = CARTESIAN_POINT ( 'NONE',  ( 0.6449049195797605938, -5.366250000000259313, 3.235821967343390337 ) ) ;
#2901 = VECTOR ( 'NONE', #2959, 1000.000000000000000 ) ;
#2902 = EDGE_CURVE ( 'NONE', #6954, #14499, #276, .T. ) ;
#2903 = CARTESIAN_POINT ( 'NONE',  ( -88.81638362644000040, 63.99516924618178848, -147.9984795835769944 ) ) ;
#2904 = DIRECTION ( 'NONE',  ( -0.4999999999999997780, 0.000000000000000000, -0.8660254037844387076 ) ) ;
#2905 = DIRECTION ( 'NONE',  ( 0.000000000000000000, 0.000000000000000000, 1.000000000000000000 ) ) ;
#2906 = LINE ( 'NONE', #10100, #15025 ) ;
#2907 = CARTESIAN_POINT ( 'NONE',  ( -0.8000000000000114797, 9.500000000000000000, 0.000000000000000000 ) ) ;
#2908 = EDGE_CURVE ( 'NONE', #13232, #11184, #4074, .T. ) ;
#2909 = DIRECTION ( 'NONE',  ( 0.000000000000000000, 0.000000000000000000, 1.000000000000000000 ) ) ;
#2910 = EDGE_LOOP ( 'NONE', ( #10609, #3507, #13262, #13277, #12712, #13912 ) ) ;
#2911 = CONICAL_SURFACE ( 'NONE', #6155, 2.500000000000002220, 1.029744258676651425 ) ;
#2912 = CARTESIAN_POINT ( 'NONE',  ( 15.50000000000000000, -0.2038245569916604938, 23.94337567297399971 ) ) ;
#2913 = EDGE_CURVE ( 'NONE', #11111, #14331, #14478, .T. ) ;
#2914 = AXIS2_PLACEMENT_3D ( 'NONE', #9835, #11006, #4962 ) ;
#2915 = ADVANCED_FACE ( 'NONE', ( #14170 ), #9501, .T. ) ;
#2916 = ORIENTED_EDGE ( 'NONE', *, *, #8205, .T. ) ;
#2917 = DIRECTION ( 'NONE',  ( 0.000000000000000000, -1.000000000000000000, -4.336808689942017736E-16 ) ) ;
#2918 = CARTESIAN_POINT ( 'NONE',  ( 2.601763032574845536, -2.140624999999891198, -3.168547547573197232 ) ) ;
#2919 = ORIENTED_EDGE ( 'NONE', *, *, #764, .T. ) ;
#2920 = DIRECTION ( 'NONE',  ( -0.000000000000000000, 0.000000000000000000, -1.000000000000000000 ) ) ;
#2921 = DIRECTION ( 'NONE',  ( -0.8660254037844482555, 0.000000000000000000, 0.4999999999999831801 ) ) ;
#2922 = AXIS2_PLACEMENT_3D ( 'NONE', #2186, #15056, #10480 ) ;
#2923 = DIRECTION ( 'NONE',  ( 1.000000000000000000, 0.000000000000000000, 0.000000000000000000 ) ) ;
#2924 = DIRECTION ( 'NONE',  ( 0.000000000000000000, 0.000000000000000000, -1.000000000000000000 ) ) ;
#2925 = DIRECTION ( 'NONE',  ( -0.000000000000000000, 1.000000000000000000, 0.000000000000000000 ) ) ;
#2926 = CARTESIAN_POINT ( 'NONE',  ( 30.00000000000000000, -5.000000000000000000, -27.00000000000000000 ) ) ;
#2927 = DIRECTION ( 'NONE',  ( 0.000000000000000000, 0.000000000000000000, -1.000000000000000000 ) ) ;
#2928 = FACE_OUTER_BOUND ( 'NONE', #12607, .T. ) ;
#2929 = SHAPE_REPRESENTATION ( 'Mounting Plate', ( #285 ), #14401 ) ;
#2930 = EDGE_LOOP ( 'NONE', ( #412, #5424, #10019, #11721 ) ) ;
#2931 =( NAMED_UNIT ( * ) SI_UNIT ( $, .STERADIAN. ) SOLID_ANGLE_UNIT ( ) );
#2932 = VERTEX_POINT ( 'NONE', #5904 ) ;
#2933 = AXIS2_PLACEMENT_3D ( 'NONE', #11028, #400, #8694 ) ;
#2934 = LINE ( 'NONE', #8821, #7053 ) ;
#2935 = CARTESIAN_POINT ( 'NONE',  ( -3.844997831300933200, -1.100624999999974429, 0.3801187285354191148 ) ) ;
#2936 = EDGE_LOOP ( 'NONE', ( #10936, #7404, #8287, #10034 ) ) ;
#2937 = DIRECTION ( 'NONE',  ( 1.000000000000000000, 2.551930889570660354E-15, 0.000000000000000000 ) ) ;
#2938 = CARTESIAN_POINT ( 'NONE',  ( -91.27438362643999881, 99.17411849586700612, -152.4984795835769944 ) ) ;
#2939 = CARTESIAN_POINT ( 'NONE',  ( -16.75000000000000000, -0.2038245569916330158, 23.22168783648699986 ) ) ;
#2940 = CONICAL_SURFACE ( 'NONE', #2190, 1732.050807568789651, 1.047197551196575871 ) ;
#2941 = DIRECTION ( 'NONE',  ( 0.000000000000000000, 1.000000000000000000, 0.000000000000000000 ) ) ;
#2942 = DIRECTION ( 'NONE',  ( -0.4999999999999832356, 0.000000000000000000, -0.8660254037844483666 ) ) ;
#2943 = CARTESIAN_POINT ( 'NONE',  ( -73.80978675135780520, 64.78624853950366003, -83.44847958357698303 ) ) ;
#2944 = ORIENTED_EDGE ( 'NONE', *, *, #2383, .F. ) ;
#2945 = DIRECTION ( 'NONE',  ( 0.000000000000000000, 0.000000000000000000, 1.000000000000000000 ) ) ;
#2946 = VERTEX_POINT ( 'NONE', #7133 ) ;
#2947 = ORIENTED_EDGE ( 'NONE', *, *, #5042, .T. ) ;
#2948 = ORIENTED_EDGE ( 'NONE', *, *, #11668, .F. ) ;
#2949 = ORIENTED_EDGE ( 'NONE', *, *, #3640, .F. ) ;
#2950 = ORIENTED_EDGE ( 'NONE', *, *, #13815, .F. ) ;
#2951 = VECTOR ( 'NONE', #269, 1000.000000000000000 ) ;
#2952 = CARTESIAN_POINT ( 'NONE',  ( 15.50000000000000000, -2.500000000000000000, -21.05662432702600029 ) ) ;
#2953 = EDGE_CURVE ( 'NONE', #3303, #9068, #10755, .T. ) ;
#2954 = CARTESIAN_POINT ( 'NONE',  ( 3.380062874710183074, -2.647499999999996856, -1.401527478686670491 ) ) ;
#2955 = CARTESIAN_POINT ( 'NONE',  ( -2.431404194366994176, 4.650702586819541295, 0.000000000000000000 ) ) ;
#2956 = CARTESIAN_POINT ( 'NONE',  ( 1.111882196364886832, -4.203124999999903189, -3.661942331401731199 ) ) ;
#2957 = CARTESIAN_POINT ( 'NONE',  ( 66.41329019055578442, 5.000000000000000000, 137.5095611191910621 ) ) ;
#2958 = ADVANCED_FACE ( 'NONE', ( #52 ), #6804, .T. ) ;
#2959 = DIRECTION ( 'NONE',  ( 0.000000000000000000, 0.000000000000000000, 1.000000000000000000 ) ) ;
#2960 = DIRECTION ( 'NONE',  ( 0.8660254037844383745, -0.5000000000000003331, 0.000000000000000000 ) ) ;
#2961 = CARTESIAN_POINT ( 'NONE',  ( -0.4147139277428218418, -1.265625000000086819, -4.195123116704944088 ) ) ;
#2962 = DIRECTION ( 'NONE',  ( -1.000000000000000000, 0.000000000000000000, 0.000000000000000000 ) ) ;
#2963 = DIRECTION ( 'NONE',  ( 0.000000000000000000, 0.000000000000000000, 1.000000000000000000 ) ) ;
#2964 = CARTESIAN_POINT ( 'NONE',  ( -86.77438362644001302, 99.17411849586700612, -145.4984795835769660 ) ) ;
#2965 = ORIENTED_EDGE ( 'NONE', *, *, #9901, .F. ) ;
#2966 = DIRECTION ( 'NONE',  ( -0.000000000000000000, -0.000000000000000000, 1.000000000000000000 ) ) ;
#2967 = VERTEX_POINT ( 'NONE', #9836 ) ;
#2968 = ORIENTED_EDGE ( 'NONE', *, *, #10785, .F. ) ;
#2969 = ORIENTED_EDGE ( 'NONE', *, *, #4892, .T. ) ;
#2970 = UNCERTAINTY_MEASURE_WITH_UNIT (LENGTH_MEASURE( 1.000000000000000082E-05 ), #10862, 'distance_accuracy_value', 'NONE');
#2971 = CARTESIAN_POINT ( 'NONE',  ( -73.64736697264537213, 89.17411849586700612, -57.99847958357699440 ) ) ;
#2972 = EDGE_CURVE ( 'NONE', #7121, #8647, #9908, .T. ) ;
#2973 = ADVANCED_FACE ( 'NONE', ( #12166 ), #7379, .T. ) ;
#2974 = CARTESIAN_POINT ( 'NONE',  ( 3.211975673186791447, -5.553749999999917364, 0.6376497042497289991 ) ) ;
#2975 = PRODUCT_DEFINITION_FORMATION_WITH_SPECIFIED_SOURCE ( 'ANY', '', #12915, .NOT_KNOWN. ) ;
#2976 = CARTESIAN_POINT ( 'NONE',  ( -84.73238362644100619, 97.99516924618178848, -147.9984795835769944 ) ) ;
#2977 = DIRECTION ( 'NONE',  ( 0.000000000000000000, 1.000000000000000000, 0.000000000000000000 ) ) ;
#2978 = CARTESIAN_POINT ( 'NONE',  ( 68.41329019055577021, 0.000000000000000000, 135.5095611191910621 ) ) ;
#2979 = CARTESIAN_POINT ( 'NONE',  ( -35.27438362644000591, 111.1741184958670061, -67.49847958357700861 ) ) ;
#2980 = CARTESIAN_POINT ( 'NONE',  ( -70.11249870063934964, 75.17411849586699191, -43.99847958365485567 ) ) ;
#2981 = CARTESIAN_POINT ( 'NONE',  ( -0.3313405146688110925, -4.850625000000119869, -3.351331461923120703 ) ) ;
#2982 = ORIENTED_EDGE ( 'NONE', *, *, #8879, .T. ) ;
#2983 = CARTESIAN_POINT ( 'NONE',  ( -12.81835358098578403, -12.60000029085423812, -8.183940086454239093 ) ) ;
#2984 = ADVANCED_FACE ( 'NONE', ( #218 ), #5125, .F. ) ;
#2985 = ITEM_DEFINED_TRANSFORMATION ( 'NONE', 'NONE', #9711,  #285 ) ;
#2986 = EDGE_LOOP ( 'NONE', ( #9007, #1571, #801, #730 ) ) ;
#2987 = CARTESIAN_POINT ( 'NONE',  ( 2.807699568699258297, -3.124999999999853895, -2.806223270957961091 ) ) ;
#2988 = VERTEX_POINT ( 'NONE', #6295 ) ;
#2989 = EDGE_CURVE ( 'NONE', #1813, #12412, #1469, .T. ) ;
#2990 = CARTESIAN_POINT ( 'NONE',  ( -1.131278458607941850, -3.702338562373107322, 3.725811129568937563 ) ) ;
#2991 = DIRECTION ( 'NONE',  ( 1.000000000000000000, -0.000000000000000000, 0.000000000000000000 ) ) ;
#2992 = EDGE_CURVE ( 'NONE', #6604, #469, #8522, .T. ) ;
#2993 = CARTESIAN_POINT ( 'NONE',  ( -53.70938362644000819, 81.46011849586699327, -83.44847958357698303 ) ) ;
#2994 = EDGE_CURVE ( 'NONE', #4969, #1406, #2633, .T. ) ;
#2995 = CARTESIAN_POINT ( 'NONE',  ( -69.77438362644001302, 79.67411849586700612, -43.99847958357699440 ) ) ;
#2996 = LINE ( 'NONE', #14922, #959 ) ;
#2997 = DIRECTION ( 'NONE',  ( -1.000000000000000000, 0.000000000000000000, 0.000000000000000000 ) ) ;
#2998 = CARTESIAN_POINT ( 'NONE',  ( 15.50000000000000000, -0.4000000000005274892, 19.20000000000052864 ) ) ;
#2999 = CARTESIAN_POINT ( 'NONE',  ( -66.62325245518700001, 97.86074886511960358, -93.49847958357699440 ) ) ;
#3000 = FACE_OUTER_BOUND ( 'NONE', #7098, .T. ) ;
#3001 = EDGE_CURVE ( 'NONE', #558, #13582, #7551, .T. ) ;
#3002 = ORIENTED_EDGE ( 'NONE', *, *, #6236, .T. ) ;
#3003 = SHAPE_REPRESENTATION_RELATIONSHIP ( 'NONE' , 'NONE' ,  #11263, #10689 ) ;
#3004 = ORIENTED_EDGE ( 'NONE', *, *, #12279, .F. ) ;
#3005 = AXIS2_PLACEMENT_3D ( 'NONE', #10201, #15010, #13715 ) ;
#3006 = CARTESIAN_POINT ( 'NONE',  ( 2.577850803773711785, 4.297149196226276224, -4.769823568025666751E-16 ) ) ;
#3007 = CARTESIAN_POINT ( 'NONE',  ( 3.730555813499152329, -1.553749999999926246, 0.7430650243616526707 ) ) ;
#3008 = ORIENTED_EDGE ( 'NONE', *, *, #1284, .F. ) ;
#3009 = EDGE_CURVE ( 'NONE', #2748, #486, #13348, .T. ) ;
#3010 = CARTESIAN_POINT ( 'NONE',  ( -69.77438362644001302, 110.1741184958670061, -152.4984795835769944 ) ) ;
#3011 = AXIS2_PLACEMENT_3D ( 'NONE', #14683, #4070, #13231 ) ;
#3012 = CIRCLE ( 'NONE', #12430, 2.000000000000001776 ) ;
#3013 = FACE_OUTER_BOUND ( 'NONE', #176, .T. ) ;
#3014 = FACE_OUTER_BOUND ( 'NONE', #9328, .T. ) ;
#3015 = CYLINDRICAL_SURFACE ( 'NONE', #6271, 0.5999999999999998668 ) ;
#3016 = EDGE_LOOP ( 'NONE', ( #1722, #13713, #11320, #6487 ) ) ;
#3017 = FACE_OUTER_BOUND ( 'NONE', #5013, .T. ) ;
#3018 = EDGE_LOOP ( 'NONE', ( #5761, #12487, #9475, #757 ) ) ;
#3019 = CIRCLE ( 'NONE', #4001, 0.2000000000005261458 ) ;
#3020 = ORIENTED_EDGE ( 'NONE', *, *, #11996, .F. ) ;
#3021 = ORIENTED_EDGE ( 'NONE', *, *, #10959, .F. ) ;
#3022 = ORIENTED_EDGE ( 'NONE', *, *, #10869, .F. ) ;
#3023 = VERTEX_POINT ( 'NONE', #11007 ) ;
#3024 = CARTESIAN_POINT ( 'NONE',  ( 0.7073082199525939640, -5.780463562373353348, 3.549031173911244341 ) ) ;
#3025 = VECTOR ( 'NONE', #12618, 1000.000000000000000 ) ;
#3026 = CARTESIAN_POINT ( 'NONE',  ( -3.456628223078394679, -2.022499999999918252, -1.432834870345867984 ) ) ;
#3027 = CARTESIAN_POINT ( 'NONE',  ( 0.000000000000000000, 0.000000000000000000, 0.000000000000000000 ) ) ;
#3028 = CARTESIAN_POINT ( 'NONE',  ( -4.034970194612536254, -2.484375000000152767, -0.3959303163385184399 ) ) ;
#3029 = CARTESIAN_POINT ( 'NONE',  ( -35.58670980944424400, 5.000000000000001776, 93.54081111919107627 ) ) ;
#3030 = CARTESIAN_POINT ( 'NONE',  ( -72.92551479769302603, 94.57411849586699759, -93.49847958357699440 ) ) ;
#3031 = VECTOR ( 'NONE', #7789, 1000.000000000000000 ) ;
#3032 = CARTESIAN_POINT ( 'NONE',  ( -3.331139167509281851, 2.239389106484336978, -3.230297714791236174 ) ) ;
#3033 = CARTESIAN_POINT ( 'NONE',  ( 2.992932217727461097, -1.124999999999971800, -2.995094308971279151 ) ) ;
#3034 = DIRECTION ( 'NONE',  ( 0.8660254037844383745, -0.5000000000000003331, 0.000000000000000000 ) ) ;
#3035 = DIRECTION ( 'NONE',  ( 1.000000000000000000, 0.000000000000000000, 0.000000000000000000 ) ) ;
#3036 = CARTESIAN_POINT ( 'NONE',  ( -44.58670980944423690, 0.000000000000000000, 137.5095611191910621 ) ) ;
#3037 = ORIENTED_EDGE ( 'NONE', *, *, #2052, .F. ) ;
#3038 = DIRECTION ( 'NONE',  ( 0.000000000000000000, 0.000000000000000000, -1.000000000000000000 ) ) ;
#3039 = TOROIDAL_SURFACE ( 'NONE', #791, 2.931404194366992400, 0.5000000000000000000 ) ;
#3040 = ORIENTED_EDGE ( 'NONE', *, *, #6334, .T. ) ;
#3041 = ORIENTED_EDGE ( 'NONE', *, *, #8495, .T. ) ;
#3042 = VERTEX_POINT ( 'NONE', #14337 ) ;
#3043 = ADVANCED_FACE ( 'NONE', ( #6068 ), #10928, .F. ) ;
#3044 = VECTOR ( 'NONE', #14550, 1000.000000000000114 ) ;
#3045 = CARTESIAN_POINT ( 'NONE',  ( 15.91242688423647955, -0.3152598339557988183, 23.70526090033903799 ) ) ;
#3046 = CARTESIAN_POINT ( 'NONE',  ( 2.709518412118975039, -5.678749999999861409, -1.809455179588198792 ) ) ;
#3047 = DIRECTION ( 'NONE',  ( 9.422394424380278809E-16, -1.000000000000000000, 0.000000000000000000 ) ) ;
#3048 = DIRECTION ( 'NONE',  ( 0.8660254037844388186, 2.210036979070413080E-15, -0.4999999999999998335 ) ) ;
#3049 = AXIS2_PLACEMENT_3D ( 'NONE', #15035, #10616, #4424 ) ;
#3050 = DIRECTION ( 'NONE',  ( 0.000000000000000000, 0.000000000000000000, -1.000000000000000000 ) ) ;
#3051 = DIRECTION ( 'NONE',  ( 0.000000000000000000, 0.000000000000000000, -1.000000000000000000 ) ) ;
#3052 = CARTESIAN_POINT ( 'NONE',  ( -0.09826241581420043503, -0.4995676945082593856, 4.080646605992279241 ) ) ;
#3053 = CIRCLE ( 'NONE', #9231, 4.499999999999997335 ) ;
#3054 = CARTESIAN_POINT ( 'NONE',  ( -2.785343681203863664, -4.991249999999938680, -1.859602269982785883 ) ) ;
#3055 = VERTEX_POINT ( 'NONE', #1394 ) ;
#3056 = CARTESIAN_POINT ( 'NONE',  ( 22.58164641901421277, -2.908542350108650476E-07, -28.96834603255778262 ) ) ;
#3057 = ADVANCED_FACE ( 'NONE', ( #3949 ), #8673, .F. ) ;
#3058 = ORIENTED_EDGE ( 'NONE', *, *, #9595, .F. ) ;
#3059 = DIRECTION ( 'NONE',  ( 0.8660254037844482555, 0.000000000000000000, 0.4999999999999831801 ) ) ;
#3060 = VECTOR ( 'NONE', #6262, 1000.000000000000114 ) ;
#3061 = ORIENTED_EDGE ( 'NONE', *, *, #224, .T. ) ;
#3062 = EDGE_CURVE ( 'NONE', #3615, #7225, #13415, .T. ) ;
#3063 = AXIS2_PLACEMENT_3D ( 'NONE', #14966, #9082, #13824 ) ;
#3064 = CARTESIAN_POINT ( 'NONE',  ( -3.736626632189893105, -2.562500000000080824, 1.546606261444747554 ) ) ;
#3065 = ORIENTED_EDGE ( 'NONE', *, *, #12568, .T. ) ;
#3066 = CARTESIAN_POINT ( 'NONE',  ( 15.50000000000000000, -0.1999999999999999556, -23.94999999999999574 ) ) ;
#3067 = CARTESIAN_POINT ( 'NONE',  ( -15.50000000000000000, -2.500000000000000000, 23.94337567297399971 ) ) ;
#3068 = DIRECTION ( 'NONE',  ( 0.000000000000000000, 1.000000000000000000, 0.000000000000000000 ) ) ;
#3069 = AXIS2_PLACEMENT_3D ( 'NONE', #8636, #2740, #3983 ) ;
#3070 = CIRCLE ( 'NONE', #15190, 2.042000000000002036 ) ;
#3071 = DIRECTION ( 'NONE',  ( -1.287488025362404182E-15, -1.000000000000000000, 0.000000000000000000 ) ) ;
#3072 = CARTESIAN_POINT ( 'NONE',  ( -52.77438362643999881, 65.17411849586700612, -145.2984795835770058 ) ) ;
#3073 = CARTESIAN_POINT ( 'NONE',  ( -78.12438362644000733, 82.17411849586700612, -80.14847958357698587 ) ) ;
#3074 = PLANE ( 'NONE',  #3638 ) ;
#3075 = ADVANCED_FACE ( 'NONE', ( #459 ), #6152, .F. ) ;
#3076 = CARTESIAN_POINT ( 'NONE',  ( -69.77438362644001302, 82.17411849586700612, -81.84847958357698872 ) ) ;
#3077 = CARTESIAN_POINT ( 'NONE',  ( 76.26492623313859553, 17.69837277024786459, 140.4057819957278355 ) ) ;
#3078 = ORIENTED_EDGE ( 'NONE', *, *, #4326, .T. ) ;
#3079 = EDGE_CURVE ( 'NONE', #8700, #14725, #13189, .T. ) ;
#3080 = CARTESIAN_POINT ( 'NONE',  ( -52.77438362644100067, 99.17411849586700612, -145.2984795835770058 ) ) ;
#3081 = EDGE_CURVE ( 'NONE', #3975, #8406, #7411, .T. ) ;
#3082 = CARTESIAN_POINT ( 'NONE',  ( -3.115386749435267610, -1.991250000000079678, -2.079980318098562542 ) ) ;
#3083 = ORIENTED_EDGE ( 'NONE', *, *, #12754, .T. ) ;
#3084 = VECTOR ( 'NONE', #14729, 1000.000000000000000 ) ;
#3085 = EDGE_CURVE ( 'NONE', #1067, #11758, #2336, .T. ) ;
#3086 = DIRECTION ( 'NONE',  ( 0.000000000000000000, 0.000000000000000000, 1.000000000000000000 ) ) ;
#3087 = CARTESIAN_POINT ( 'NONE',  ( 2.598076211353311127, 1.678847577293378190, 4.500000000000000000 ) ) ;
#3088 =( NAMED_UNIT ( * ) SI_UNIT ( $, .STERADIAN. ) SOLID_ANGLE_UNIT ( ) );
#3089 = CARTESIAN_POINT ( 'NONE',  ( -35.58670980944424400, 5.000000000000001776, 101.4783111191910621 ) ) ;
#3090 = VECTOR ( 'NONE', #13017, 1000.000000000000000 ) ;
#3091 = EDGE_CURVE ( 'NONE', #6403, #7923, #9012, .T. ) ;
#3092 = CARTESIAN_POINT ( 'NONE',  ( -52.77438362644000591, 99.17411849586700612, -86.49847958357699440 ) ) ;
#3093 = ORIENTED_EDGE ( 'NONE', *, *, #14175, .T. ) ;
#3094 = CARTESIAN_POINT ( 'NONE',  ( -15.50000000000000000, -2.500000000000000000, 23.94337567297399971 ) ) ;
#3095 = VERTEX_POINT ( 'NONE', #9123 ) ;
#3096 = EDGE_CURVE ( 'NONE', #11342, #14750, #4601, .T. ) ;
#3097 = VERTEX_POINT ( 'NONE', #7894 ) ;
#3098 = EDGE_CURVE ( 'NONE', #5984, #9369, #6594, .T. ) ;
#3099 = ORIENTED_EDGE ( 'NONE', *, *, #10446, .F. ) ;
#3100 = ORIENTED_EDGE ( 'NONE', *, *, #11526, .T. ) ;
#3101 = VERTEX_POINT ( 'NONE', #10203 ) ;
#3102 = CARTESIAN_POINT ( 'NONE',  ( -0.3539834606290251928, -5.733588562373254760, 3.607703032259661935 ) ) ;
#3103 = STYLED_ITEM ( 'NONE', ( #3532 ), #357 ) ;
#3104 = CARTESIAN_POINT ( 'NONE',  ( 1.843713500184339216, -0.7568749999999383471, -3.447171040406491027 ) ) ;
#3105 = CIRCLE ( 'NONE', #869, 4.000000000000000888 ) ;
#3106 = CYLINDRICAL_SURFACE ( 'NONE', #3606, 3.499999999999999556 ) ;
#3107 = AXIS2_PLACEMENT_3D ( 'NONE', #13596, #2726, #3897 ) ;
#3108 = CARTESIAN_POINT ( 'NONE',  ( 2.225207906715364281, -2.843749999999932943, 3.332158947996217702 ) ) ;
#3109 = LINE ( 'NONE', #546, #7766 ) ;
#3110 = CARTESIAN_POINT ( 'NONE',  ( -86.77438362644001302, 59.67411849586700612, -15.85886927678779834 ) ) ;
#3111 = CARTESIAN_POINT ( 'NONE',  ( 2.801070059014833191, 1.881841424954898923, 4.148404342226347907 ) ) ;
#3112 = CARTESIAN_POINT ( 'NONE',  ( 4.232448940998905229, -0.9843749999998714362, 0.4153177470904050317 ) ) ;
#3113 = FACE_OUTER_BOUND ( 'NONE', #15171, .T. ) ;
#3114 = CARTESIAN_POINT ( 'NONE',  ( -101.2743836264399988, 57.67411849586699901, -79.49847958357700861 ) ) ;
#3115 = CARTESIAN_POINT ( 'NONE',  ( -91.02438362644100778, 99.17411849586700612, -145.4984795835769660 ) ) ;
#3116 = VERTEX_POINT ( 'NONE', #2939 ) ;
#3117 = CARTESIAN_POINT ( 'NONE',  ( -62.02799568714584666, 164.3482369917340122, -152.4984795835769944 ) ) ;
#3118 = ORIENTED_EDGE ( 'NONE', *, *, #11866, .F. ) ;
#3119 = AXIS2_PLACEMENT_3D ( 'NONE', #11137, #6576, #11291 ) ;
#3120 = ORIENTED_EDGE ( 'NONE', *, *, #12195, .T. ) ;
#3121 = ORIENTED_EDGE ( 'NONE', *, *, #12172, .T. ) ;
#3122 = CIRCLE ( 'NONE', #11786, 0.2000000000005226763 ) ;
#3123 = DIRECTION ( 'NONE',  ( 0.08715574274766123286, 0.000000000000000000, -0.9961946980917453232 ) ) ;
#3124 = CARTESIAN_POINT ( 'NONE',  ( -3.196762997434627440, -4.147500000000007958, 1.325534829466321840 ) ) ;
#3125 = DIRECTION ( 'NONE',  ( 1.000000000000000000, 0.000000000000000000, 0.000000000000000000 ) ) ;
#3126 = AXIS2_PLACEMENT_3D ( 'NONE', #4051, #11261, #14742 ) ;
#3127 = CARTESIAN_POINT ( 'NONE',  ( 2.093999815491831562, 9.250000000000001776, 0.000000000000000000 ) ) ;
#3128 = CARTESIAN_POINT ( 'NONE',  ( -50.27438362644100067, 59.67411849586700612, -79.59847958357700293 ) ) ;
#3129 = AXIS2_PLACEMENT_3D ( 'NONE', #4519, #2109, #10246 ) ;
#3130 = PLANE ( 'NONE',  #9851 ) ;
#3131 = CARTESIAN_POINT ( 'NONE',  ( -0.3199098613971397276, -0.4995676945082599407, 4.077077341688482015 ) ) ;
#3132 = VECTOR ( 'NONE', #6499, 1000.000000000000000 ) ;
#3133 = LINE ( 'NONE', #4683, #9272 ) ;
#3134 = CARTESIAN_POINT ( 'NONE',  ( -1.562933739280453205, -5.256875000000181153, 2.922265072135110220 ) ) ;
#3135 = ORIENTED_EDGE ( 'NONE', *, *, #7997, .F. ) ;
#3136 = PLANE ( 'NONE',  #14285 ) ;
#3137 = ORIENTED_EDGE ( 'NONE', *, *, #3174, .T. ) ;
#3138 = CARTESIAN_POINT ( 'NONE',  ( 17.12895037488186389, -3.654606557864051197, 0.2687305842673423095 ) ) ;
#3139 = AXIS2_PLACEMENT_3D ( 'NONE', #8657, #7438, #14552 ) ;
#3140 = VERTEX_POINT ( 'NONE', #677 ) ;
#3141 = AXIS2_PLACEMENT_3D ( 'NONE', #5752, #10454, #10618 ) ;
#3142 = CARTESIAN_POINT ( 'NONE',  ( -0.4147139277428218418, -1.265625000000086819, -4.195123116704944088 ) ) ;
#3143 = ORIENTED_EDGE ( 'NONE', *, *, #1189, .F. ) ;
#3144 = CARTESIAN_POINT ( 'NONE',  ( 3.305159631054613634, -3.092963562373059805, -2.207179784781822196 ) ) ;
#3145 = DIRECTION ( 'NONE',  ( 0.000000000000000000, -1.734723475976807686E-15, -1.000000000000000000 ) ) ;
#3146 = ADVANCED_FACE ( 'NONE', ( #1921 ), #13574, .T. ) ;
#3147 = DIRECTION ( 'NONE',  ( 0.000000000000000000, 0.000000000000000000, -1.000000000000000000 ) ) ;
#3148 = CARTESIAN_POINT ( 'NONE',  ( -50.73238362644099197, 97.99516924618178848, -147.9984795835769944 ) ) ;
#3149 = CIRCLE ( 'NONE', #5131, 8.000000000000007105 ) ;
#3150 = ADVANCED_FACE ( 'NONE', ( #1766 ), #12330, .F. ) ;
#3151 = VECTOR ( 'NONE', #14959, 1000.000000000000000 ) ;
#3152 = DIRECTION ( 'NONE',  ( 0.000000000000000000, 0.000000000000000000, -1.000000000000000000 ) ) ;
#3153 = DIRECTION ( 'NONE',  ( -9.422394424380278809E-16, 1.000000000000000000, -0.000000000000000000 ) ) ;
#3154 = CARTESIAN_POINT ( 'NONE',  ( -71.73429801879703405, 98.05590563058170517, -94.29040204287990434 ) ) ;
#3155 = CARTESIAN_POINT ( 'NONE',  ( 1.634139617129772404, 11.99999970914575798, -0.3335879563140091153 ) ) ;
#3156 =( NAMED_UNIT ( * ) PLANE_ANGLE_UNIT ( ) SI_UNIT ( $, .RADIAN. ) );
#3157 = EDGE_LOOP ( 'NONE', ( #14083, #3657 ) ) ;
#3158 = CARTESIAN_POINT ( 'NONE',  ( -3.516205069202407163, -0.1631249999999115075, 1.881096664271727059 ) ) ;
#3159 = VERTEX_POINT ( 'NONE', #12404 ) ;
#3160 = CIRCLE ( 'NONE', #13804, 4.250000000000003553 ) ;
#3161 = ADVANCED_FACE ( 'NONE', ( #12559 ), #8903, .F. ) ;
#3162 = ADVANCED_FACE ( 'NONE', ( #14859 ), #13971, .T. ) ;
#3163 = CARTESIAN_POINT ( 'NONE',  ( -57.27438362644000591, 65.17411849586700612, -86.49847958357699440 ) ) ;
#3164 = CARTESIAN_POINT ( 'NONE',  ( -46.58670980944423690, 5.000000000000000000, 135.5095611191910621 ) ) ;
#3165 = CYLINDRICAL_SURFACE ( 'NONE', #5325, 17.85000000000000497 ) ;
#3166 = AXIS2_PLACEMENT_3D ( 'NONE', #4916, #3502, #4981 ) ;
#3167 = EDGE_LOOP ( 'NONE', ( #9997, #3866, #4139, #11739 ) ) ;
#3168 = FACE_OUTER_BOUND ( 'NONE', #3259, .T. ) ;
#3169 = ORIENTED_EDGE ( 'NONE', *, *, #6418, .T. ) ;
#3170 = ADVANCED_FACE ( 'NONE', ( #4329 ), #11460, .F. ) ;
#3171 = ORIENTED_EDGE ( 'NONE', *, *, #7647, .T. ) ;
#3172 = CARTESIAN_POINT ( 'NONE',  ( 0.6449049195797814660, -5.366250000000259313, 3.235821967343390781 ) ) ;
#3173 = ORIENTED_EDGE ( 'NONE', *, *, #7761, .F. ) ;
#3174 = EDGE_CURVE ( 'NONE', #51, #4925, #1695, .T. ) ;
#3175 = VERTEX_POINT ( 'NONE', #7753 ) ;
#3176 = VERTEX_POINT ( 'NONE', #11308 ) ;
#3177 = CARTESIAN_POINT ( 'NONE',  ( -13.41835358098578723, -12.00000029085423137, -56.77834603255778489 ) ) ;
#3178 = CARTESIAN_POINT ( 'NONE',  ( -1.487946254897619447, -0.8975000000000187272, -3.594883137563858355 ) ) ;
#3179 = ADVANCED_FACE ( 'NONE', ( #9051 ), #12993, .F. ) ;
#3180 = CIRCLE ( 'NONE', #1197, 2.000000000000001776 ) ;
#3181 = DIRECTION ( 'NONE',  ( 0.000000000000000000, 0.000000000000000000, -1.000000000000000000 ) ) ;
#3182 = CARTESIAN_POINT ( 'NONE',  ( 3.986138996993924266, -2.999999999999990674, -0.001451045610905104914 ) ) ;
#3183 = DIRECTION ( 'NONE',  ( -1.000000000000000000, 0.000000000000000000, 0.000000000000000000 ) ) ;
#3184 = DIRECTION ( 'NONE',  ( 0.000000000000000000, 0.000000000000000000, -1.000000000000000000 ) ) ;
#3185 = EDGE_CURVE ( 'NONE', #8073, #4888, #4404, .T. ) ;
#3186 = EDGE_CURVE ( 'NONE', #8760, #5254, #14713, .T. ) ;
#3187 = DIRECTION ( 'NONE',  ( -1.000000000000000000, 0.000000000000000000, 0.000000000000000000 ) ) ;
#3188 = DIRECTION ( 'NONE',  ( 1.000000000000000000, 1.541976423090494894E-16, 0.000000000000000000 ) ) ;
#3189 = DIRECTION ( 'NONE',  ( 1.000000000000000000, 0.000000000000000000, 0.000000000000000000 ) ) ;
#3190 = DIRECTION ( 'NONE',  ( -1.000000000000000000, 0.000000000000000000, 0.000000000000000000 ) ) ;
#3191 = ORIENTED_EDGE ( 'NONE', *, *, #12541, .T. ) ;
#3192 = DIRECTION ( 'NONE',  ( 0.000000000000000000, 1.000000000000000000, 0.000000000000000000 ) ) ;
#3193 = ORIENTED_EDGE ( 'NONE', *, *, #11871, .T. ) ;
#3194 = AXIS2_PLACEMENT_3D ( 'NONE', #9053, #13794, #1989 ) ;
#3195 = EDGE_CURVE ( 'NONE', #12756, #7247, #11649, .T. ) ;
#3196 = ORIENTED_EDGE ( 'NONE', *, *, #10348, .F. ) ;
#3197 = ORIENTED_EDGE ( 'NONE', *, *, #7968, .T. ) ;
#3198 = DIRECTION ( 'NONE',  ( 0.000000000000000000, 0.000000000000000000, -1.000000000000000000 ) ) ;
#3199 = CARTESIAN_POINT ( 'NONE',  ( 3.151910583997929116, -4.522499999999531894, 1.304188709559700232 ) ) ;
#3200 = EDGE_CURVE ( 'NONE', #11913, #9286, #4101, .T. ) ;
#3201 = DIRECTION ( 'NONE',  ( 1.000000000000000000, 0.000000000000000000, 0.000000000000000000 ) ) ;
#3202 = CARTESIAN_POINT ( 'NONE',  ( -86.77438362644001302, 65.17411849586700612, -86.49847958357699440 ) ) ;
#3203 = CARTESIAN_POINT ( 'NONE',  ( -86.77438362643999881, 65.17411849586700612, -145.4984795835769944 ) ) ;
#3204 = DIRECTION ( 'NONE',  ( 0.000000000000000000, 0.000000000000000000, -1.000000000000000000 ) ) ;
#3205 = CARTESIAN_POINT ( 'NONE',  ( -102.2743836264399988, 65.17411849586700612, -15.85886927678779834 ) ) ;
#3206 = DIRECTION ( 'NONE',  ( 0.000000000000000000, 0.000000000000000000, -1.000000000000000000 ) ) ;
#3207 = ORIENTED_EDGE ( 'NONE', *, *, #5948, .F. ) ;
#3208 = CYLINDRICAL_SURFACE ( 'NONE', #6647, 1.785937500000001066 ) ;
#3209 = ORIENTED_EDGE ( 'NONE', *, *, #14709, .T. ) ;
#3210 = DIRECTION ( 'NONE',  ( 1.000000000000000000, 0.000000000000000000, 0.000000000000000000 ) ) ;
#3211 = ORIENTED_EDGE ( 'NONE', *, *, #4281, .F. ) ;
#3212 = EDGE_LOOP ( 'NONE', ( #10829, #3241 ) ) ;
#3213 = CARTESIAN_POINT ( 'NONE',  ( -2.783274248898092385, -3.374213562373101105, -2.784736148173822201 ) ) ;
#3214 = CARTESIAN_POINT ( 'NONE',  ( 21.98164641901421135, -2.908542394189813650E-07, 0.2664120436859911956 ) ) ;
#3215 = DIRECTION ( 'NONE',  ( 0.000000000000000000, -1.000000000000000000, 0.000000000000000000 ) ) ;
#3216 = DIRECTION ( 'NONE',  ( -0.7071067811865425767, 0.000000000000000000, -0.7071067811865525687 ) ) ;
#3217 = CARTESIAN_POINT ( 'NONE',  ( 33.35543536254877495, -3.618985300545106920, 6.000000000000000000 ) ) ;
#3218 = CARTESIAN_POINT ( 'NONE',  ( -71.99490031521868616, 98.02122612623958275, -94.16161080865532540 ) ) ;
#3219 = DIRECTION ( 'NONE',  ( -1.747085166004344019E-15, 1.000000000000000000, -0.000000000000000000 ) ) ;
#3220 = APPLICATION_PROTOCOL_DEFINITION ( 'draft international standard', 'automotive_design', 1998, #11690 ) ;
#3221 = EDGE_LOOP ( 'NONE', ( #8785, #58, #4258 ) ) ;
#3222 =( LENGTH_UNIT ( ) NAMED_UNIT ( * ) SI_UNIT ( .MILLI., .METRE. ) );
#3223 = CARTESIAN_POINT ( 'NONE',  ( -1.070211464245647282, -5.296874999999768185, -3.523343936188056968 ) ) ;
#3224 = ORIENTED_EDGE ( 'NONE', *, *, #13873, .T. ) ;
#3225 = EDGE_CURVE ( 'NONE', #11747, #13723, #6074, .T. ) ;
#3226 = CARTESIAN_POINT ( 'NONE',  ( -0.7073002561900942897, -2.866249999999988418, -3.560643744722076232 ) ) ;
#3227 = CARTESIAN_POINT ( 'NONE',  ( -1.733190484027920863, 0.04649911033017210121, -4.499999999999999112 ) ) ;
#3228 = CARTESIAN_POINT ( 'NONE',  ( 10.02391400960032009, -11.00000029085428110, 70.00595460678397330 ) ) ;
#3229 = DIRECTION ( 'NONE',  ( 0.000000000000000000, 0.000000000000000000, 1.000000000000000000 ) ) ;
#3230 = CARTESIAN_POINT ( 'NONE',  ( 57.41329019055577021, 5.000000000000000000, 129.5095611191910621 ) ) ;
#3231 = DIRECTION ( 'NONE',  ( 0.000000000000000000, 1.000000000000000000, 0.000000000000000000 ) ) ;
#3232 = CARTESIAN_POINT ( 'NONE',  ( -102.2743836264264132, 104.6741184958692088, -79.59847958357700293 ) ) ;
#3233 = ORIENTED_EDGE ( 'NONE', *, *, #13222, .T. ) ;
#3234 = CYLINDRICAL_SURFACE ( 'NONE', #10744, 2.500000000000002220 ) ;
#3235 = PRODUCT_DEFINITION ( 'UNKNOWN', '', #4274, #778 ) ;
#3236 = ADVANCED_FACE ( 'NONE', ( #14015 ), #7301, .F. ) ;
#3237 = VERTEX_POINT ( 'NONE', #9423 ) ;
#3238 = ORIENTED_EDGE ( 'NONE', *, *, #125, .T. ) ;
#3239 = CARTESIAN_POINT ( 'NONE',  ( 2.393563981450126388, -4.710000000000058584, -2.395350030107681327 ) ) ;
#3240 = ORIENTED_EDGE ( 'NONE', *, *, #9252, .F. ) ;
#3241 = ORIENTED_EDGE ( 'NONE', *, *, #8769, .T. ) ;
#3242 = ORIENTED_EDGE ( 'NONE', *, *, #576, .F. ) ;
#3243 = VECTOR ( 'NONE', #340, 1000.000000000000000 ) ;
#3244 = CARTESIAN_POINT ( 'NONE',  ( 3.441012398922143056, -5.952338562373084230, 1.044788167591881534 ) ) ;
#3245 = CARTESIAN_POINT ( 'NONE',  ( 3.852585042300790352, -0.6162500000000914469, -0.7652758215885018256 ) ) ;
#3246 = AXIS2_PLACEMENT_3D ( 'NONE', #8670, #5344, #6292 ) ;
#3247 = CARTESIAN_POINT ( 'NONE',  ( -9.503456061879925088, 11.99999970914574021, 69.60114695342350899 ) ) ;
#3248 = CARTESIAN_POINT ( 'NONE',  ( 3.946741062051739579, -1.953124999999941380, 1.198372487375103157 ) ) ;
#3249 = DIRECTION ( 'NONE',  ( 1.000000000000000000, 0.000000000000000000, 0.000000000000000000 ) ) ;
#3250 = DIRECTION ( 'NONE',  ( 0.000000000000000000, 0.000000000000000000, -1.000000000000000000 ) ) ;
#3251 = LINE ( 'NONE', #12880, #1689 ) ;
#3252 = DIRECTION ( 'NONE',  ( 0.000000000000000000, 1.000000000000000000, 0.000000000000000000 ) ) ;
#3253 = DIRECTION ( 'NONE',  ( 1.000000000000000000, 8.284258017326334836E-16, 0.000000000000000000 ) ) ;
#3254 = DIRECTION ( 'NONE',  ( 0.000000000000000000, 0.000000000000000000, 1.000000000000000000 ) ) ;
#3255 = ORIENTED_EDGE ( 'NONE', *, *, #1865, .F. ) ;
#3256 = FACE_OUTER_BOUND ( 'NONE', #11408, .T. ) ;
#3257 = EDGE_CURVE ( 'NONE', #7951, #11859, #8526, .T. ) ;
#3258 = AXIS2_PLACEMENT_3D ( 'NONE', #2196, #9100, #10257 ) ;
#3259 = EDGE_LOOP ( 'NONE', ( #9270, #10468, #12809, #130 ) ) ;
#3260 = ORIENTED_EDGE ( 'NONE', *, *, #13886, .T. ) ;
#3261 = CIRCLE ( 'NONE', #543, 3.173335668876520188 ) ;
#3262 = ADVANCED_FACE ( 'NONE', ( #14241 ), #7960, .F. ) ;
#3263 =( REPRESENTATION_RELATIONSHIP ('NONE','NONE', #13541, #12357 ) REPRESENTATION_RELATIONSHIP_WITH_TRANSFORMATION ( #4075 )SHAPE_REPRESENTATION_RELATIONSHIP( ) );
#3264 = DIRECTION ( 'NONE',  ( 0.7071067811865474617, 0.000000000000000000, 0.7071067811865474617 ) ) ;
#3265 = EDGE_CURVE ( 'NONE', #777, #10300, #3568, .T. ) ;
#3266 = CARTESIAN_POINT ( 'NONE',  ( -3.325293793763300698, -4.038125000000090559, -1.009645679448947231 ) ) ;
#3267 = CIRCLE ( 'NONE', #548, 2.042000000000002036 ) ;
#3268 = DIRECTION ( 'NONE',  ( 0.000000000000000000, 0.000000000000000000, 1.000000000000000000 ) ) ;
#3269 = CARTESIAN_POINT ( 'NONE',  ( -50.02438362644000591, 99.17411849586700612, -145.4984795835769944 ) ) ;
#3270 = DIRECTION ( 'NONE',  ( -1.000000000000000000, -0.000000000000000000, -0.000000000000000000 ) ) ;
#3271 = CYLINDRICAL_SURFACE ( 'NONE', #10302, 2.750000000000002665 ) ;
#3272 = VECTOR ( 'NONE', #11574, 1000.000000000000000 ) ;
#3273 = EDGE_CURVE ( 'NONE', #6326, #957, #11846, .T. ) ;
#3274 = FACE_OUTER_BOUND ( 'NONE', #2121, .T. ) ;
#3275 = CARTESIAN_POINT ( 'NONE',  ( -69.77438362644002723, 75.17411849587348627, -43.99847958364158984 ) ) ;
#3276 = DIRECTION ( 'NONE',  ( -1.287488025362404182E-15, -1.000000000000000000, 0.000000000000000000 ) ) ;
#3277 = CONICAL_SURFACE ( 'NONE', #14421, 3.750000000000003553, 0.7853981633974476129 ) ;
#3278 = ORIENTED_EDGE ( 'NONE', *, *, #14074, .F. ) ;
#3279 = CARTESIAN_POINT ( 'NONE',  ( 2.093999815491831562, 9.500000000000001776, 0.000000000000000000 ) ) ;
#3280 = EDGE_CURVE ( 'NONE', #12826, #12970, #2324, .T. ) ;
#3281 = VERTEX_POINT ( 'NONE', #8126 ) ;
#3282 = VECTOR ( 'NONE', #4331, 1000.000000000000000 ) ;
#3283 = ORIENTED_EDGE ( 'NONE', *, *, #13299, .F. ) ;
#3284 = DIRECTION ( 'NONE',  ( 0.000000000000000000, -0.000000000000000000, 1.000000000000000000 ) ) ;
#3285 = EDGE_LOOP ( 'NONE', ( #4934, #11509, #7518, #3988 ) ) ;
#3286 = CARTESIAN_POINT ( 'NONE',  ( 3.275404563695782034, -1.109375000000065503, -2.686596450795923463 ) ) ;
#3287 = ORIENTED_EDGE ( 'NONE', *, *, #10080, .T. ) ;
#3288 = AXIS2_PLACEMENT_3D ( 'NONE', #9143, #8061, #10308 ) ;
#3289 = CARTESIAN_POINT ( 'NONE',  ( 3.173589072176457027, -2.108588562373159725, -2.603092057013398186 ) ) ;
#3290 = DIRECTION ( 'NONE',  ( 0.000000000000000000, 1.047133521511407648E-16, 1.000000000000000000 ) ) ;
#3291 = CARTESIAN_POINT ( 'NONE',  ( -82.27438362643999881, 65.17411849586700612, -145.4984795835769660 ) ) ;
#3292 = AXIS2_PLACEMENT_3D ( 'NONE', #12543, #2925, #9967 ) ;
#3293 = CARTESIAN_POINT ( 'NONE',  ( 14.25000000000000000, -0.2038245569916330158, -23.22168783648699986 ) ) ;
#3294 = DIRECTION ( 'NONE',  ( -0.000000000000000000, -4.336808689942017736E-16, 1.000000000000000000 ) ) ;
#3295 = LINE ( 'NONE', #10502, #9831 ) ;
#3296 = VECTOR ( 'NONE', #6657, 1000.000000000000000 ) ;
#3297 = AXIS2_PLACEMENT_3D ( 'NONE', #1087, #14047, #12887 ) ;
#3298 = DIRECTION ( 'NONE',  ( -1.000000000000000000, 0.000000000000000000, 0.000000000000000000 ) ) ;
#3299 = ORIENTED_EDGE ( 'NONE', *, *, #610, .F. ) ;
#3300 = CIRCLE ( 'NONE', #11738, 4.250000000000003553 ) ;
#3301 =( NAMED_UNIT ( * ) SI_UNIT ( $, .STERADIAN. ) SOLID_ANGLE_UNIT ( ) );
#3302 = CARTESIAN_POINT ( 'NONE',  ( 3.654380903460823671, -4.968749999999916511, 0.7255053565382596492 ) ) ;
#3303 = VERTEX_POINT ( 'NONE', #5898 ) ;
#3304 = CARTESIAN_POINT ( 'NONE',  ( 2.337649614532405717, -2.444375000000051479, 2.849939602875970035 ) ) ;
#3305 = CARTESIAN_POINT ( 'NONE',  ( -66.62325245518700001, 94.57411849586699759, -93.49847958357699440 ) ) ;
#3306 = CIRCLE ( 'NONE', #4805, 16.00000000000000000 ) ;
#3307 = DIRECTION ( 'NONE',  ( 0.000000000000000000, 0.000000000000000000, -1.000000000000000000 ) ) ;
#3308 = PLANE ( 'NONE',  #5327 ) ;
#3309 = TOROIDAL_SURFACE ( 'NONE', #5561, 2.400000000000000355, 0.6000000000000000888 ) ;
#3310 = FACE_OUTER_BOUND ( 'NONE', #12128, .T. ) ;
#3311 = DIRECTION ( 'NONE',  ( 0.000000000000000000, -0.000000000000000000, 1.000000000000000000 ) ) ;
#3312 = EDGE_CURVE ( 'NONE', #3902, #3610, #6819, .T. ) ;
#3313 = CARTESIAN_POINT ( 'NONE',  ( -3.466497813382189541, -5.275048774667015827, -7.182839392716466875E-16 ) ) ;
#3314 = ORIENTED_EDGE ( 'NONE', *, *, #3098, .T. ) ;
#3315 = DIRECTION ( 'NONE',  ( 0.000000000000000000, -0.1666666666666656582, 0.9860132971832695770 ) ) ;
#3316 = AXIS2_PLACEMENT_3D ( 'NONE', #13432, #7622, #7547 ) ;
#3317 = AXIS2_PLACEMENT_3D ( 'NONE', #3228, #10060, #8977 ) ;
#3318 = ORIENTED_EDGE ( 'NONE', *, *, #7161, .F. ) ;
#3319 = ORIENTED_EDGE ( 'NONE', *, *, #6690, .F. ) ;
#3320 = CARTESIAN_POINT ( 'NONE',  ( 2.619799856955865369, -4.694374999999869402, -2.148899555557211904 ) ) ;
#3321 = ORIENTED_EDGE ( 'NONE', *, *, #12384, .T. ) ;
#3322 = EDGE_LOOP ( 'NONE', ( #4478, #12052, #6178, #5192 ) ) ;
#3323 = EDGE_LOOP ( 'NONE', ( #14803, #9020, #9557, #8069 ) ) ;
#3324 = DIRECTION ( 'NONE',  ( 0.000000000000000000, 1.000000000000000000, 0.000000000000000000 ) ) ;
#3325 = CARTESIAN_POINT ( 'NONE',  ( -2.463482987169076210, -0.9443750000000532552, -3.003366100166337649 ) ) ;
#3326 = DIRECTION ( 'NONE',  ( 0.000000000000000000, 1.000000000000000000, 0.000000000000000000 ) ) ;
#3327 = CARTESIAN_POINT ( 'NONE',  ( 3.808142666863014281, -3.046875000000033751, -1.156701755244785801 ) ) ;
#3328 = CIRCLE ( 'NONE', #8294, 2.700000000000001066 ) ;
#3329 = DIRECTION ( 'NONE',  ( 0.000000000000000000, 1.000000000000000000, 0.000000000000000000 ) ) ;
#3330 = ADVANCED_FACE ( 'NONE', ( #10670 ), #3308, .T. ) ;
#3331 = CARTESIAN_POINT ( 'NONE',  ( -4.993158575045113956, 1.881841424954880937, 0.3515956577736513711 ) ) ;
#3332 = CARTESIAN_POINT ( 'NONE',  ( -4.296251640119561621, -0.4995676945082693776, 0.01637110057554332782 ) ) ;
#3333 = DIRECTION ( 'NONE',  ( 0.000000000000000000, 1.000000000000000000, 0.000000000000000000 ) ) ;
#3334 = CARTESIAN_POINT ( 'NONE',  ( 15.50000000000000000, -0.2038245569916604938, -21.05662432702600029 ) ) ;
#3335 = EDGE_CURVE ( 'NONE', #11131, #9085, #7313, .T. ) ;
#3336 = CARTESIAN_POINT ( 'NONE',  ( -69.77438362644001302, 82.17411849586700612, -80.44847958357698303 ) ) ;
#3337 = EDGE_LOOP ( 'NONE', ( #300, #6266, #10072, #13106, #9826 ) ) ;
#3338 = FACE_BOUND ( 'NONE', #7783, .T. ) ;
#3339 = EDGE_LOOP ( 'NONE', ( #990, #2733, #3004, #13618 ) ) ;
#3340 = ORIENTED_EDGE ( 'NONE', *, *, #11042, .T. ) ;
#3341 = EDGE_LOOP ( 'NONE', ( #12495, #9657, #5611, #7391 ) ) ;
#3342 = CIRCLE ( 'NONE', #7605, 4.250000000000003553 ) ;
#3343 = CARTESIAN_POINT ( 'NONE',  ( -86.77438362644100778, 99.17411849586700612, -147.9984795835769944 ) ) ;
#3344 = CIRCLE ( 'NONE', #12028, 2.500000000000002220 ) ;
#3345 = CARTESIAN_POINT ( 'NONE',  ( 2.393563981450126388, -4.710000000000058584, -2.395350030107596506 ) ) ;
#3346 = SURFACE_STYLE_FILL_AREA ( #13973 ) ;
#3347 = CARTESIAN_POINT ( 'NONE',  ( 3.897114317029974462, 9.945166405816860437E-15, 2.249999999999999556 ) ) ;
#3348 = DIRECTION ( 'NONE',  ( -0.3469356515732558988, -0.9378889346118975956, 0.000000000000000000 ) ) ;
#3349 = EDGE_CURVE ( 'NONE', #4841, #9681, #44, .T. ) ;
#3350 = CARTESIAN_POINT ( 'NONE',  ( 15.50000000000000000, -1.037157890325000054, 22.50000000000000000 ) ) ;
#3351 = LINE ( 'NONE', #945, #10594 ) ;
#3352 = VECTOR ( 'NONE', #15153, 1000.000000000000000 ) ;
#3353 = CARTESIAN_POINT ( 'NONE',  ( -14.25000000000000000, -2.500000000000000000, 21.77831216351300014 ) ) ;
#3354 = EDGE_CURVE ( 'NONE', #5205, #4633, #10510, .T. ) ;
#3355 = B_SPLINE_CURVE_WITH_KNOTS ( 'NONE', 3,
 ( #932, #1166, #4433, #11640, #10546, #5691 ),
 .UNSPECIFIED., .F., .F.,
 ( 4, 2, 4 ),
 ( 0.0002380763768115301549, 0.7291065797294569162, 1.457975083082102330 ),
 .UNSPECIFIED. ) ;
#3356 = DIRECTION ( 'NONE',  ( 0.000000000000000000, -1.000000000000000000, 0.000000000000000000 ) ) ;
#3357 = ORIENTED_EDGE ( 'NONE', *, *, #14266, .F. ) ;
#3358 = VECTOR ( 'NONE', #13721, 1000.000000000000000 ) ;
#3359 = DIRECTION ( 'NONE',  ( 1.000000000000000000, 0.000000000000000000, 0.000000000000000000 ) ) ;
#3360 = EDGE_LOOP ( 'NONE', ( #12573, #15118, #5472, #6061 ) ) ;
#3361 = ORIENTED_EDGE ( 'NONE', *, *, #580, .F. ) ;
#3362 = CARTESIAN_POINT ( 'NONE',  ( -86.77438362643999881, 62.81621999649657084, -147.9984795835769944 ) ) ;
#3363 = VERTEX_POINT ( 'NONE', #5662 ) ;
#3364 = ADVANCED_FACE ( 'NONE', ( #2149 ), #2348, .T. ) ;
#3365 = CARTESIAN_POINT ( 'NONE',  ( 3.298003658611986744, -0.8906249999999793499, 2.704611316345772121 ) ) ;
#3366 = ORIENTED_EDGE ( 'NONE', *, *, #2138, .F. ) ;
#3367 = CIRCLE ( 'NONE', #5873, 4.296275033669348709 ) ;
#3368 = CARTESIAN_POINT ( 'NONE',  ( -2.190848337519055278, -3.342963562373078457, -3.276249760082800222 ) ) ;
#3369 = VECTOR ( 'NONE', #354, 1000.000000000000114 ) ;
#3370 = AXIS2_PLACEMENT_3D ( 'NONE', #10192, #6660, #11446 ) ;
#3371 = DIRECTION ( 'NONE',  ( 0.000000000000000000, 0.000000000000000000, 1.000000000000000000 ) ) ;
#3372 = EDGE_CURVE ( 'NONE', #9550, #10808, #12933, .T. ) ;
#3373 = CARTESIAN_POINT ( 'NONE',  ( 15.50000000000000000, -0.1999999999999999556, 22.50000000000000000 ) ) ;
#3374 = CARTESIAN_POINT ( 'NONE',  ( 4.993158575045104186, 1.881841424954905362, -0.3515956577736533140 ) ) ;
#3375 = EDGE_CURVE ( 'NONE', #13570, #4529, #1135, .T. ) ;
#3376 = CYLINDRICAL_SURFACE ( 'NONE', #10164, 4.250000000000003553 ) ;
#3377 = EDGE_CURVE ( 'NONE', #134, #6145, #9032, .T. ) ;
#3378 = ORIENTED_EDGE ( 'NONE', *, *, #6444, .T. ) ;
#3379 = AXIS2_PLACEMENT_3D ( 'NONE', #14621, #9656, #8221 ) ;
#3380 = FACE_OUTER_BOUND ( 'NONE', #4823, .T. ) ;
#3381 = DIRECTION ( 'NONE',  ( 0.000000000000000000, 0.000000000000000000, 1.000000000000000000 ) ) ;
#3382 = AXIS2_PLACEMENT_3D ( 'NONE', #6463, #10879, #9773 ) ;
#3383 = ORIENTED_EDGE ( 'NONE', *, *, #12083, .F. ) ;
#3384 = CARTESIAN_POINT ( 'NONE',  ( -14.66242688423474227, -0.3152598339554810170, 21.54019739087905094 ) ) ;
#3385 = CARTESIAN_POINT ( 'NONE',  ( 0.7624512442115695121, -0.8037500000000172840, -3.827857439461599398 ) ) ;
#3386 = ORIENTED_EDGE ( 'NONE', *, *, #9660, .F. ) ;
#3387 = CIRCLE ( 'NONE', #3890, 1.999999999999989564 ) ;
#3388 = CARTESIAN_POINT ( 'NONE',  ( -1.707523105661799434, -2.913124999999936904, -3.196535590052164810 ) ) ;
#3389 = TOROIDAL_SURFACE ( 'NONE', #14045, 2.700000000000000178, 0.2000000000000000111 ) ;
#3390 = DIRECTION ( 'NONE',  ( 0.000000000000000000, 0.000000000000000000, 1.000000000000000000 ) ) ;
#3391 = CARTESIAN_POINT ( 'NONE',  ( 2.931404194366990623, 4.650702586819546624, 3.589934763638662607E-16 ) ) ;
#3392 = CARTESIAN_POINT ( 'NONE',  ( -89.47438362644099641, 99.17411849586700612, -145.4984795835769944 ) ) ;
#3393 = CARTESIAN_POINT ( 'NONE',  ( -86.77438362644001302, 82.17411849586700612, -3.496191900462991775 ) ) ;
#3394 = ORIENTED_EDGE ( 'NONE', *, *, #2029, .F. ) ;
#3395 = CARTESIAN_POINT ( 'NONE',  ( -69.77438362644001302, 82.17411849586700612, -117.9984795835769944 ) ) ;
#3396 = AXIS2_PLACEMENT_3D ( 'NONE', #2983, #13549, #10106 ) ;
#3397 = EDGE_LOOP ( 'NONE', ( #2159, #13691, #2537, #364 ) ) ;
#3398 = CIRCLE ( 'NONE', #10837, 1.000000000000000888 ) ;
#3399 = VERTEX_POINT ( 'NONE', #9736 ) ;
#3400 = CARTESIAN_POINT ( 'NONE',  ( -0.9979582191392041279, -4.288125000000008846, 3.294238300096191896 ) ) ;
#3401 = VERTEX_POINT ( 'NONE', #11922 ) ;
#3402 = ORIENTED_EDGE ( 'NONE', *, *, #230, .F. ) ;
#3403 = ORIENTED_EDGE ( 'NONE', *, *, #10051, .T. ) ;
#3404 = CARTESIAN_POINT ( 'NONE',  ( -0.7460806596055710171, -4.280463562373175712, -3.743634425862352177 ) ) ;
#3405 = CARTESIAN_POINT ( 'NONE',  ( -86.77438362644001302, 65.17411849586700612, -86.49847958357699440 ) ) ;
#3406 = DIRECTION ( 'NONE',  ( 0.000000000000000000, 0.000000000000000000, -1.000000000000000000 ) ) ;
#3407 = CARTESIAN_POINT ( 'NONE',  ( -89.47438362644099641, 99.17411849586700612, -145.2984795835770058 ) ) ;
#3408 = CARTESIAN_POINT ( 'NONE',  ( -42.77438362644000591, 104.6741184958670061, -79.59847958357700293 ) ) ;
#3409 = CARTESIAN_POINT ( 'NONE',  ( -4.296227084909979510, -0.4995677573761841406, -0.01166785054812304046 ) ) ;
#3410 = CARTESIAN_POINT ( 'NONE',  ( 35.35543536254876074, -3.618985300545107364, 0.000000000000000000 ) ) ;
#3411 = PLANE ( 'NONE',  #116 ) ;
#3412 = FACE_OUTER_BOUND ( 'NONE', #14216, .T. ) ;
#3413 = CARTESIAN_POINT ( 'NONE',  ( -2.348309169242665639, -5.210000000000155396, 2.347120911809276400 ) ) ;
#3414 = LINE ( 'NONE', #6991, #14452 ) ;
#3415 = EDGE_LOOP ( 'NONE', ( #299, #92, #8912 ) ) ;
#3416 = DIRECTION ( 'NONE',  ( 0.8660254037844383745, -0.5000000000000003331, 0.000000000000000000 ) ) ;
#3417 = ORIENTED_EDGE ( 'NONE', *, *, #9660, .T. ) ;
#3418 =( BOUNDED_CURVE ( )  B_SPLINE_CURVE ( 3, ( #2971, #8631, #7410, #1727 ),
 .UNSPECIFIED., .F., .F. ) 
 B_SPLINE_CURVE_WITH_KNOTS ( ( 4, 4 ),
 ( 5.777824796895650650, 6.283185307179590673 ),
 .UNSPECIFIED. ) 
 CURVE ( )  GEOMETRIC_REPRESENTATION_ITEM ( )  RATIONAL_B_SPLINE_CURVE ( ( 1.000000000000000000, 0.9788305577012550440, 0.9788305577012550440, 1.000000000000000000 ) ) 
 REPRESENTATION_ITEM ( '' )  );
#3419 = ORIENTED_EDGE ( 'NONE', *, *, #9949, .T. ) ;
#3420 = ORIENTED_EDGE ( 'NONE', *, *, #9575, .T. ) ;
#3421 = EDGE_CURVE ( 'NONE', #12869, #9247, #13168, .T. ) ;
#3422 = AXIS2_PLACEMENT_3D ( 'NONE', #530, #7681, #13350 ) ;
#3423 = CARTESIAN_POINT ( 'NONE',  ( 0.000000000000000000, 0.000000000000000000, 0.000000000000000000 ) ) ;
#3424 = CARTESIAN_POINT ( 'NONE',  ( 3.388605160257775140, -4.569374999999831211, 0.3324735777646720680 ) ) ;
#3425 = EDGE_CURVE ( 'NONE', #9134, #15255, #12151, .T. ) ;
#3426 = DIRECTION ( 'NONE',  ( -0.000000000000000000, 1.000000000000000000, -0.000000000000000000 ) ) ;
#3427 = FACE_OUTER_BOUND ( 'NONE', #8897, .T. ) ;
#3428 = DIRECTION ( 'NONE',  ( 1.000000000000000000, 0.000000000000000000, 0.000000000000000000 ) ) ;
#3429 = FACE_OUTER_BOUND ( 'NONE', #6924, .T. ) ;
#3430 = CARTESIAN_POINT ( 'NONE',  ( -70.11249870063895173, 89.17411849586699191, -43.99847958365485567 ) ) ;
#3431 = DIRECTION ( 'NONE',  ( -0.000000000000000000, -0.000000000000000000, 1.000000000000000000 ) ) ;
#3432 = DIRECTION ( 'NONE',  ( 0.000000000000000000, 0.000000000000000000, 1.000000000000000000 ) ) ;
#3433 = VECTOR ( 'NONE', #9504, 1000.000000000000000 ) ;
#3434 = ORIENTED_EDGE ( 'NONE', *, *, #4000, .T. ) ;
#3435 = CARTESIAN_POINT ( 'NONE',  ( 21.98164641901421135, -11.40000029085423705, -11.73358795631401463 ) ) ;
#3436 = ORIENTED_EDGE ( 'NONE', *, *, #14642, .T. ) ;
#3437 = VERTEX_POINT ( 'NONE', #9652 ) ;
#3438 = DIRECTION ( 'NONE',  ( -1.000000000000000000, 0.000000000000000000, 0.000000000000000000 ) ) ;
#3439 = PRODUCT_RELATED_PRODUCT_CATEGORY ( 'part', '', ( #7112 ) ) ;
#3440 = ADVANCED_FACE ( 'NONE', ( #5104 ), #14473, .T. ) ;
#3441 = ORIENTED_EDGE ( 'NONE', *, *, #13981, .T. ) ;
#3442 = CARTESIAN_POINT ( 'NONE',  ( 1.243192046278082774, -0.7968750000001610934, 4.092941397521737912 ) ) ;
#3443 = EDGE_LOOP ( 'NONE', ( #6400, #8612, #14866 ) ) ;
#3444 = CARTESIAN_POINT ( 'NONE',  ( 4.101399898226999241, -1.983588562372964770, 0.4024520375143380568 ) ) ;
#3445 = AXIS2_PLACEMENT_3D ( 'NONE', #13700, #12684, #3071 ) ;
#3446 = CARTESIAN_POINT ( 'NONE',  ( -13.41835358098578723, -2.908542394189813650E-07, 0.2664120436859911956 ) ) ;
#3447 = CYLINDRICAL_SURFACE ( 'NONE', #327, 0.6000000000000000888 ) ;
#3448 = EDGE_CURVE ( 'NONE', #4566, #5234, #120, .T. ) ;
#3449 = FACE_OUTER_BOUND ( 'NONE', #15256, .T. ) ;
#3450 = ORIENTED_EDGE ( 'NONE', *, *, #9487, .F. ) ;
#3451 = CARTESIAN_POINT ( 'NONE',  ( 15.50000000000000000, -2.500000000000000000, 21.05662432702600029 ) ) ;
#3452 = CARTESIAN_POINT ( 'NONE',  ( -90.85838362644000199, 65.17411849586700612, -147.9984795835769944 ) ) ;
#3453 = EDGE_CURVE ( 'NONE', #12945, #1628, #4872, .T. ) ;
#3454 = VERTEX_POINT ( 'NONE', #13249 ) ;
#3455 = CYLINDRICAL_SURFACE ( 'NONE', #15233, 10.49999999999999467 ) ;
#3456 = CARTESIAN_POINT ( 'NONE',  ( -0.001357705120208648440, -5.249999999999984013, -3.688496797837457652 ) ) ;
#3457 = ORIENTED_EDGE ( 'NONE', *, *, #6136, .F. ) ;
#3458 = EDGE_CURVE ( 'NONE', #15330, #13910, #6129, .T. ) ;
#3459 = EDGE_CURVE ( 'NONE', #13870, #14415, #7068, .T. ) ;
#3460 = CARTESIAN_POINT ( 'NONE',  ( -2.795825449145424191, -2.975624999999864517, -2.292747793747622609 ) ) ;
#3461 = LINE ( 'NONE', #8191, #8943 ) ;
#3462 = PLANE ( 'NONE',  #2156 ) ;
#3463 = DIRECTION ( 'NONE',  ( 0.000000000000000000, 0.000000000000000000, 1.000000000000000000 ) ) ;
#3464 = ADVANCED_FACE ( 'NONE', ( #3626, #3857 ), #1603, .T. ) ;
#3465 = DIRECTION ( 'NONE',  ( 1.000000000000000000, 2.551930889570660354E-15, 0.000000000000000000 ) ) ;
#3466 = DIRECTION ( 'NONE',  ( -0.8660254037844482555, 0.000000000000000000, -0.4999999999999831801 ) ) ;
#3467 = DIRECTION ( 'NONE',  ( 1.000000000000000000, -0.000000000000000000, 0.000000000000000000 ) ) ;
#3468 = LINE ( 'NONE', #12864, #11195 ) ;
#3469 = EDGE_LOOP ( 'NONE', ( #10073, #12787, #12414, #152 ) ) ;
#3470 = CARTESIAN_POINT ( 'NONE',  ( -53.79538362644100147, 97.40569462133919387, -147.9984795835769944 ) ) ;
#3471 = ADVANCED_FACE ( 'NONE', ( #8503 ), #1448, .F. ) ;
#3472 = ORIENTED_EDGE ( 'NONE', *, *, #3091, .T. ) ;
#3473 = VERTEX_POINT ( 'NONE', #1520 ) ;
#3474 = CARTESIAN_POINT ( 'NONE',  ( -3.325293793763386851, -4.038125000000090559, -1.009645679448947453 ) ) ;
#3475 = ORIENTED_EDGE ( 'NONE', *, *, #11238, .T. ) ;
#3476 = ORIENTED_EDGE ( 'NONE', *, *, #8867, .T. ) ;
#3477 = ORIENTED_EDGE ( 'NONE', *, *, #3185, .T. ) ;
#3478 = CARTESIAN_POINT ( 'NONE',  ( 2.714559208474450980, -4.124213562372948338, -2.713141310347332968 ) ) ;
#3479 = CARTESIAN_POINT ( 'NONE',  ( -69.77438362644001302, 82.17411849586700612, -80.14847958357698587 ) ) ;
#3480 = DIRECTION ( 'NONE',  ( 0.000000000000000000, -1.000000000000000000, 0.000000000000000000 ) ) ;
#3481 = CARTESIAN_POINT ( 'NONE',  ( -50.73238362644099197, 100.3530677455522238, -147.9984795835769944 ) ) ;
#3482 = FACE_OUTER_BOUND ( 'NONE', #15277, .T. ) ;
#3483 = DIRECTION ( 'NONE',  ( 1.000000000000000000, 0.000000000000000000, 0.000000000000000000 ) ) ;
#3484 = CARTESIAN_POINT ( 'NONE',  ( -86.77438362643999881, 65.17411849586700612, -145.4984795835769944 ) ) ;
#3485 = CARTESIAN_POINT ( 'NONE',  ( 15.50000000000000000, -2.500000000000000000, 21.05662432702600029 ) ) ;
#3486 = DIRECTION ( 'NONE',  ( 0.000000000000000000, 0.000000000000000000, -1.000000000000000000 ) ) ;
#3487 = CARTESIAN_POINT ( 'NONE',  ( -2.103997734759339711, -5.225624999999808118, 2.565685703212198021 ) ) ;
#3488 = DIRECTION ( 'NONE',  ( 0.000000000000000000, 0.000000000000000000, -1.000000000000000000 ) ) ;
#3489 = ORIENTED_EDGE ( 'NONE', *, *, #11200, .F. ) ;
#3490 = CARTESIAN_POINT ( 'NONE',  ( -53.77438362644000591, 82.17411849586700612, -183.7533135795160320 ) ) ;
#3491 = VERTEX_POINT ( 'NONE', #2756 ) ;
#3492 = AXIS2_PLACEMENT_3D ( 'NONE', #7653, #10974, #1352 ) ;
#3493 = ORIENTED_EDGE ( 'NONE', *, *, #10855, .F. ) ;
#3494 = ORIENTED_EDGE ( 'NONE', *, *, #13886, .F. ) ;
#3495 = AXIS2_PLACEMENT_3D ( 'NONE', #5580, #4783, #1050 ) ;
#3496 = DIRECTION ( 'NONE',  ( 0.000000000000000000, 0.000000000000000000, 1.000000000000000000 ) ) ;
#3497 = CARTESIAN_POINT ( 'NONE',  ( -2.557519727433407386, -2.960000000000007958, -2.558839988362045403 ) ) ;
#3498 = FACE_OUTER_BOUND ( 'NONE', #10090, .T. ) ;
#3499 = CARTESIAN_POINT ( 'NONE',  ( -14.24999999999999822, -0.2715193793361453389, 22.98718409945082541 ) ) ;
#3500 = PLANE ( 'NONE',  #7107 ) ;
#3501 = AXIS2_PLACEMENT_3D ( 'NONE', #10113, #8956, #7506 ) ;
#3502 = DIRECTION ( 'NONE',  ( 1.000000000000000000, -1.287488025362404182E-15, 0.000000000000000000 ) ) ;
#3503 = CARTESIAN_POINT ( 'NONE',  ( 26.34657265215283317, 5.000000000000000000, 89.50956111919107627 ) ) ;
#3504 = DIRECTION ( 'NONE',  ( 0.000000000000000000, 0.000000000000000000, 1.000000000000000000 ) ) ;
#3505 = LINE ( 'NONE', #1104, #8498 ) ;
#3506 = VECTOR ( 'NONE', #6254, 1000.000000000000000 ) ;
#3507 = ORIENTED_EDGE ( 'NONE', *, *, #7893, .T. ) ;
#3508 = DIRECTION ( 'NONE',  ( 0.000000000000000000, 0.000000000000000000, 1.000000000000000000 ) ) ;
#3509 = CIRCLE ( 'NONE', #15143, 3.499999999999999556 ) ;
#3510 = EDGE_CURVE ( 'NONE', #632, #7802, #9768, .T. ) ;
#3511 = VERTEX_POINT ( 'NONE', #7433 ) ;
#3512 = ORIENTED_EDGE ( 'NONE', *, *, #4710, .F. ) ;
#3513 = FACE_OUTER_BOUND ( 'NONE', #14123, .T. ) ;
#3514 = VECTOR ( 'NONE', #4745, 1000.000000000000000 ) ;
#3515 = CARTESIAN_POINT ( 'NONE',  ( 1.688254324138965146, 0.1874999999998931965, 4.071669181187491660 ) ) ;
#3516 = VERTEX_POINT ( 'NONE', #10759 ) ;
#3517 = CARTESIAN_POINT ( 'NONE',  ( 3.546006434268102137, -0.9054635623730455940, 2.367515899259258649 ) ) ;
#3518 = AXIS2_PLACEMENT_3D ( 'NONE', #13108, #2536, #14392 ) ;
#3519 = DIRECTION ( 'NONE',  ( 0.000000000000000000, 0.000000000000000000, 1.000000000000000000 ) ) ;
#3520 = DIRECTION ( 'NONE',  ( 0.9961946980917452121, -3.779777825264101491E-17, 0.08715574274766160756 ) ) ;
#3521 = FACE_OUTER_BOUND ( 'NONE', #13096, .T. ) ;
#3522 = ADVANCED_FACE ( 'NONE', ( #7356 ), #2590, .F. ) ;
#3523 = MECHANICAL_DESIGN_GEOMETRIC_PRESENTATION_REPRESENTATION (  '', ( #11956 ), #11209 ) ;
#3524 = DIRECTION ( 'NONE',  ( 0.000000000000000000, 0.000000000000000000, -1.000000000000000000 ) ) ;
#3525 = ORIENTED_EDGE ( 'NONE', *, *, #6710, .T. ) ;
#3526 = PLANE ( 'NONE',  #11808 ) ;
#3527 = ADVANCED_FACE ( 'NONE', ( #8358 ), #11271, .F. ) ;
#3528 = CARTESIAN_POINT ( 'NONE',  ( -62.02799568714584666, 103.6741184958669919, -79.59847958357700293 ) ) ;
#3529 = VECTOR ( 'NONE', #5143, 1000.000000000000114 ) ;
#3530 = PRODUCT_CONTEXT ( 'NONE', #12500, 'mechanical' ) ;
#3531 = ORIENTED_EDGE ( 'NONE', *, *, #518, .F. ) ;
#3532 = PRESENTATION_STYLE_ASSIGNMENT (( #9647 ) ) ;
#3533 = CARTESIAN_POINT ( 'NONE',  ( -3.249648180954406662, -3.593749999999990230, 2.170113394669044293 ) ) ;
#3534 = EDGE_LOOP ( 'NONE', ( #5590, #3008, #12588, #11899, #9005 ) ) ;
#3535 = AXIS2_PLACEMENT_3D ( 'NONE', #444, #5182, #9891 ) ;
#3536 = CARTESIAN_POINT ( 'NONE',  ( 3.667419683216786908, -2.585000000000003517, 0.0009491222189788412963 ) ) ;
#3537 = AXIS2_PLACEMENT_3D ( 'NONE', #14957, #10145, #4350 ) ;
#3538 = EDGE_CURVE ( 'NONE', #1459, #3615, #6086, .T. ) ;
#3539 = CARTESIAN_POINT ( 'NONE',  ( 21.98164641901421135, -12.00000029085423670, -11.73358795631400930 ) ) ;
#3540 = AXIS2_PLACEMENT_3D ( 'NONE', #1402, #3574, #295 ) ;
#3541 = DIRECTION ( 'NONE',  ( 0.000000000000000000, -0.9922779949676268085, -0.1240337885538713436 ) ) ;
#3542 = LINE ( 'NONE', #11618, #10711 ) ;
#3543 = DIRECTION ( 'NONE',  ( 0.000000000000000000, -1.000000000000000000, 0.000000000000000000 ) ) ;
#3544 = EDGE_CURVE ( 'NONE', #13723, #3787, #268, .T. ) ;
#3545 = DIRECTION ( 'NONE',  ( 0.000000000000000000, 0.000000000000000000, 1.000000000000000000 ) ) ;
#3546 = TOROIDAL_SURFACE ( 'NONE', #12986, 11.50000000000000000, 1.000000000000000000 ) ;
#3547 = ORIENTED_EDGE ( 'NONE', *, *, #11519, .T. ) ;
#3548 = DIRECTION ( 'NONE',  ( -9.422394424380278809E-16, 1.000000000000000000, -0.000000000000000000 ) ) ;
#3549 = ORIENTED_EDGE ( 'NONE', *, *, #5714, .F. ) ;
#3550 = FACE_OUTER_BOUND ( 'NONE', #4649, .T. ) ;
#3551 = CARTESIAN_POINT ( 'NONE',  ( -1.336190917661153943, -3.897499999999990195, -3.228188129988408761 ) ) ;
#3552 = ORIENTED_EDGE ( 'NONE', *, *, #9609, .F. ) ;
#3553 = ORIENTED_EDGE ( 'NONE', *, *, #8440, .F. ) ;
#3554 = AXIS2_PLACEMENT_3D ( 'NONE', #9130, #11693, #1059 ) ;
#3555 = ORIENTED_EDGE ( 'NONE', *, *, #9402, .F. ) ;
#3556 = CARTESIAN_POINT ( 'NONE',  ( 0.3733708913940425034, -4.233588562373078901, -3.805181778647142465 ) ) ;
#3557 = ADVANCED_FACE ( 'NONE', ( #14547 ), #356, .F. ) ;
#3558 = FACE_OUTER_BOUND ( 'NONE', #2827, .T. ) ;
#3559 = CIRCLE ( 'NONE', #7285, 5.499999999999998224 ) ;
#3560 = PLANE ( 'NONE',  #5640 ) ;
#3561 = DIRECTION ( 'NONE',  ( -1.000000000000000000, 0.000000000000000000, 0.000000000000000000 ) ) ;
#3562 = EDGE_CURVE ( 'NONE', #10261, #6610, #11423, .T. ) ;
#3563 = PLANE ( 'NONE',  #10828 ) ;
#3564 = CARTESIAN_POINT ( 'NONE',  ( -69.77438362644001302, 82.17411849586700612, -44.99847958359070788 ) ) ;
#3565 = DIRECTION ( 'NONE',  ( 1.000000000000000000, 0.000000000000000000, 0.000000000000000000 ) ) ;
#3566 = CARTESIAN_POINT ( 'NONE',  ( -38.27438362644000591, 114.1741184958670061, -79.49847958357700861 ) ) ;
#3567 = AXIS2_PLACEMENT_3D ( 'NONE', #13683, #9017, #13758 ) ;
#3568 = CIRCLE ( 'NONE', #1094, 1.449999999999999956 ) ;
#3569 = CARTESIAN_POINT ( 'NONE',  ( 3.535094671665813593, -3.584999999999991083, -0.001309597400350119394 ) ) ;
#3570 = ADVANCED_FACE ( 'NONE', ( #11582 ), #6713, .T. ) ;
#3571 = LINE ( 'NONE', #13045, #15181 ) ;
#3572 = EDGE_CURVE ( 'NONE', #4992, #4558, #12012, .T. ) ;
#3573 = VERTEX_POINT ( 'NONE', #7935 ) ;
#3574 = DIRECTION ( 'NONE',  ( 0.000000000000000000, 0.000000000000000000, 1.000000000000000000 ) ) ;
#3575 = ORIENTED_EDGE ( 'NONE', *, *, #8103, .F. ) ;
#3576 = ORIENTED_EDGE ( 'NONE', *, *, #1865, .T. ) ;
#3577 = VERTEX_POINT ( 'NONE', #11355 ) ;
#3578 = CLOSED_SHELL ( 'NONE', ( #5437, #13207, #14077, #11920, #13533, #6618, #15206, #9409, #4234, #3170, #13609, #3744, #1479, #6595, #2524 ) ) ;
#3579 = VECTOR ( 'NONE', #759, 1000.000000000000000 ) ;
#3580 = CARTESIAN_POINT ( 'NONE',  ( 3.039561480324906029, -2.678749999999966214, -2.029833227700108544 ) ) ;
#3581 = AXIS2_PLACEMENT_3D ( 'NONE', #13836, #4447, #868 ) ;
#3582 = DIRECTION ( 'NONE',  ( 0.000000000000000000, 0.000000000000000000, 1.000000000000000000 ) ) ;
#3583 = B_SPLINE_CURVE_WITH_KNOTS ( 'NONE', 3,
 ( #13446, #2889, #7636, #12356, #10886, #2807, #4920, #1496 ),
 .UNSPECIFIED., .F., .F.,
 ( 4, 2, 2, 4 ),
 ( 0.04105254269951062740, 0.04300721795512758849, 0.04398455558293606904, 0.04496189321074454959 ),
 .UNSPECIFIED. ) ;
#3584 = DIRECTION ( 'NONE',  ( 2.551930889570659960E-15, -1.000000000000000000, -0.000000000000000000 ) ) ;
#3585 = DIRECTION ( 'NONE',  ( 1.000000000000000000, 0.000000000000000000, 0.000000000000000000 ) ) ;
#3586 = LINE ( 'NONE', #2185, #2137 ) ;
#3587 = CARTESIAN_POINT ( 'NONE',  ( -12.81835358098578403, 11.99999970914576686, -14.73358795631400575 ) ) ;
#3588 = DIRECTION ( 'NONE',  ( -0.000000000000000000, 1.000000000000000000, -0.000000000000000000 ) ) ;
#3589 = DIRECTION ( 'NONE',  ( 0.8660254037844383745, -0.5000000000000003331, 0.000000000000000000 ) ) ;
#3590 = DIRECTION ( 'NONE',  ( 0.000000000000000000, 0.000000000000000000, -1.000000000000000000 ) ) ;
#3591 = DIRECTION ( 'NONE',  ( -1.000000000000000000, -2.551930889570659960E-15, 0.000000000000000000 ) ) ;
#3592 = ORIENTED_EDGE ( 'NONE', *, *, #1668, .T. ) ;
#3593 = CARTESIAN_POINT ( 'NONE',  ( -15.50000000000000000, -2.500000000000000000, -23.94337567297399971 ) ) ;
#3594 = AXIS2_PLACEMENT_3D ( 'NONE', #3080, #8740, #4174 ) ;
#3595 = EDGE_LOOP ( 'NONE', ( #2874, #3705 ) ) ;
#3596 = EDGE_LOOP ( 'NONE', ( #6060, #11134 ) ) ;
#3597 = VERTEX_POINT ( 'NONE', #7588 ) ;
#3598 = AXIS2_PLACEMENT_3D ( 'NONE', #5688, #9078, #7915 ) ;
#3599 = LINE ( 'NONE', #1339, #5253 ) ;
#3600 = CARTESIAN_POINT ( 'NONE',  ( -3.816972974264043028, -0.4218749999999791833, -2.038447964682808422 ) ) ;
#3601 = ORIENTED_EDGE ( 'NONE', *, *, #1535, .T. ) ;
#3602 = CARTESIAN_POINT ( 'NONE',  ( -2.644124373199357336, -1.639838562373160169, 3.220131994730173197 ) ) ;
#3603 = VECTOR ( 'NONE', #11374, 1000.000000000000000 ) ;
#3604 = CARTESIAN_POINT ( 'NONE',  ( -15.91242688423473517, -0.3152598339554900653, 21.29473909965994594 ) ) ;
#3605 = DIRECTION ( 'NONE',  ( 0.000000000000000000, 1.000000000000000000, 0.000000000000000000 ) ) ;
#3606 = AXIS2_PLACEMENT_3D ( 'NONE', #13657, #761, #1782 ) ;
#3607 = CARTESIAN_POINT ( 'NONE',  ( -13.41835358098578723, -11.40000029085424238, 0.2664120436859911956 ) ) ;
#3608 = VECTOR ( 'NONE', #9506, 1000.000000000000000 ) ;
#3609 = CYLINDRICAL_SURFACE ( 'NONE', #9682, 2.000000000000001776 ) ;
#3610 = VERTEX_POINT ( 'NONE', #6862 ) ;
#3611 = CARTESIAN_POINT ( 'NONE',  ( -84.73238362643999722, 66.35306774555222376, -147.9984795835769944 ) ) ;
#3612 = CARTESIAN_POINT ( 'NONE',  ( 16.75451632270442559, 11.78522852589359537, 0.2672856210392292042 ) ) ;
#3613 = AXIS2_PLACEMENT_3D ( 'NONE', #8399, #2656, #1495 ) ;
#3614 = PRODUCT_CONTEXT ( 'NONE', #11997, 'mechanical' ) ;
#3615 = VERTEX_POINT ( 'NONE', #790 ) ;
#3616 = CIRCLE ( 'NONE', #653, 4.499999999999997335 ) ;
#3617 = LINE ( 'NONE', #1206, #5348 ) ;
#3618 = CARTESIAN_POINT ( 'NONE',  ( -3.787710864223658991, -4.499999999999990230, 0.001388818612877307929 ) ) ;
#3619 = VERTEX_POINT ( 'NONE', #14979 ) ;
#3620 = AXIS2_PLACEMENT_3D ( 'NONE', #1055, #9359, #8278 ) ;
#3621 = ADVANCED_FACE ( 'NONE', ( #9095 ), #947, .T. ) ;
#3622 = CARTESIAN_POINT ( 'NONE',  ( -2.746234728672232173, -0.9599999999999920819, -2.744228674164098436 ) ) ;
#3623 = EDGE_CURVE ( 'NONE', #13986, #8154, #2037, .T. ) ;
#3624 = LINE ( 'NONE', #267, #7083 ) ;
#3625 = CARTESIAN_POINT ( 'NONE',  ( -84.02438362643999881, 99.17411849586700612, -86.49847958357699440 ) ) ;
#3626 = FACE_BOUND ( 'NONE', #11532, .T. ) ;
#3627 = AXIS2_PLACEMENT_3D ( 'NONE', #3203, #6641, #6559 ) ;
#3628 = DIRECTION ( 'NONE',  ( 0.8660254037844383745, -0.5000000000000003331, 0.000000000000000000 ) ) ;
#3629 = CARTESIAN_POINT ( 'NONE',  ( -84.73238362644100619, 100.3530677455522238, -150.4984795835770228 ) ) ;
#3630 = PRESENTATION_LAYER_ASSIGNMENT (  '', '', ( #10058 ) ) ;
#3631 = DIRECTION ( 'NONE',  ( 0.000000000000000000, 0.000000000000000000, -1.000000000000000000 ) ) ;
#3632 = ORIENTED_EDGE ( 'NONE', *, *, #13246, .F. ) ;
#3633 = DIRECTION ( 'NONE',  ( 0.000000000000000000, 0.000000000000000000, 1.000000000000000000 ) ) ;
#3634 = VERTEX_POINT ( 'NONE', #6784 ) ;
#3635 = FACE_OUTER_BOUND ( 'NONE', #7157, .T. ) ;
#3636 = CARTESIAN_POINT ( 'NONE',  ( 1.412068586280953220, -2.397499999999971099, 3.411535633775466980 ) ) ;
#3637 = ORIENTED_EDGE ( 'NONE', *, *, #2031, .T. ) ;
#3638 = AXIS2_PLACEMENT_3D ( 'NONE', #13564, #6500, #7812 ) ;
#3639 = ORIENTED_EDGE ( 'NONE', *, *, #13072, .F. ) ;
#3640 = EDGE_CURVE ( 'NONE', #6308, #7951, #13984, .T. ) ;
#3641 = EDGE_LOOP ( 'NONE', ( #11917, #6041, #5187, #570, #2592, #2713 ) ) ;
#3642 = AXIS2_PLACEMENT_3D ( 'NONE', #1393, #8293, #7066 ) ;
#3643 = DIRECTION ( 'NONE',  ( 2.065146995210485003E-17, 4.251773225433349175E-17, 1.000000000000000000 ) ) ;
#3644 = CARTESIAN_POINT ( 'NONE',  ( -69.77438362644001302, 82.17411849586700612, -79.49847958357700861 ) ) ;
#3645 = CARTESIAN_POINT ( 'NONE',  ( -16.75000000000000000, -2.500000000000000000, 23.22168783648699986 ) ) ;
#3646 = CARTESIAN_POINT ( 'NONE',  ( -4.296274425956841725, -0.5002988223950231017, 0.02453012155904704325 ) ) ;
#3647 = VECTOR ( 'NONE', #11584, 1000.000000000000114 ) ;
#3648 = DIRECTION ( 'NONE',  ( 1.000000000000000000, 0.000000000000000000, 0.000000000000000000 ) ) ;
#3649 = CARTESIAN_POINT ( 'NONE',  ( 2.743301530724824744, -3.475625000000028386, 2.252549412313605615 ) ) ;
#3650 = LINE ( 'NONE', #11566, #2063 ) ;
#3651 = EDGE_CURVE ( 'NONE', #7228, #3097, #15058, .T. ) ;
#3652 = ORIENTED_EDGE ( 'NONE', *, *, #5539, .F. ) ;
#3653 = EDGE_CURVE ( 'NONE', #840, #10550, #2841, .T. ) ;
#3654 = SPHERICAL_SURFACE ( 'NONE', #2296, 0.8600000000000014300 ) ;
#3655 = EDGE_LOOP ( 'NONE', ( #8071, #2478, #9762, #13732 ) ) ;
#3656 = ORIENTED_EDGE ( 'NONE', *, *, #8641, .F. ) ;
#3657 = ORIENTED_EDGE ( 'NONE', *, *, #12344, .T. ) ;
#3658 = EDGE_CURVE ( 'NONE', #11018, #5594, #8088, .T. ) ;
#3659 = DIRECTION ( 'NONE',  ( -0.9999934663667180423, 1.567696289299852607E-18, -0.003614861529252313879 ) ) ;
#3660 = EDGE_CURVE ( 'NONE', #1915, #14331, #14617, .T. ) ;
#3661 = AXIS2_PLACEMENT_3D ( 'NONE', #6010, #3817, #8543 ) ;
#3662 = CARTESIAN_POINT ( 'NONE',  ( 57.41329019055577021, 0.000000000000000000, 99.29549861919106490 ) ) ;
#3663 = LINE ( 'NONE', #4831, #7002 ) ;
#3664 = DIRECTION ( 'NONE',  ( -0.8660254037844387076, -0.4999999999999998890, 0.000000000000000000 ) ) ;
#3665 = CARTESIAN_POINT ( 'NONE',  ( 14.25000000000000000, -2.500000000000000000, -23.22168783648699986 ) ) ;
#3666 = CARTESIAN_POINT ( 'NONE',  ( 22.58164641901421632, -12.00000029085423137, -56.77834603255778489 ) ) ;
#3667 = DIRECTION ( 'NONE',  ( 0.000000000000000000, 4.336808689942017736E-16, -1.000000000000000000 ) ) ;
#3668 = DIRECTION ( 'NONE',  ( 0.000000000000000000, 0.000000000000000000, -1.000000000000000000 ) ) ;
#3669 = DIRECTION ( 'NONE',  ( 0.000000000000000000, 0.1240337885538713436, -0.9922779949676268085 ) ) ;
#3670 = DIRECTION ( 'NONE',  ( 0.000000000000000000, -1.000000000000000000, -4.336808689942017736E-16 ) ) ;
#3671 = ADVANCED_FACE ( 'NONE', ( #1890 ), #366, .F. ) ;
#3672 = EDGE_LOOP ( 'NONE', ( #4415, #5112, #13654, #8594 ) ) ;
#3673 = FACE_OUTER_BOUND ( 'NONE', #8685, .T. ) ;
#3674 = ORIENTED_EDGE ( 'NONE', *, *, #2407, .F. ) ;
#3675 = CIRCLE ( 'NONE', #937, 16.50000000000000000 ) ;
#3676 = ORIENTED_EDGE ( 'NONE', *, *, #12273, .F. ) ;
#3677 = ADVANCED_FACE ( 'NONE', ( #1964 ), #5703, .F. ) ;
#3678 = CARTESIAN_POINT ( 'NONE',  ( -2.749513137126650353, -0.3593750000000536238, -3.352117812333079705 ) ) ;
#3679 = ORIENTED_EDGE ( 'NONE', *, *, #13981, .F. ) ;
#3680 = CARTESIAN_POINT ( 'NONE',  ( -3.489569499876165271, -1.405463562373098663, -2.332997265744571447 ) ) ;
#3681 = CARTESIAN_POINT ( 'NONE',  ( -16.75000000000000000, -0.2038245569916330158, 21.77831216351300014 ) ) ;
#3682 = CARTESIAN_POINT ( 'NONE',  ( -88.81638362644000040, 65.17411849586700612, -147.9984795835769944 ) ) ;
#3683 = CONICAL_SURFACE ( 'NONE', #6912, 2.042000000000002036, 1.047197551196596965 ) ;
#3684 = DIRECTION ( 'NONE',  ( -0.000000000000000000, -0.000000000000000000, 1.000000000000000000 ) ) ;
#3685 = DIRECTION ( 'NONE',  ( -1.000000000000000000, 0.000000000000000000, 0.000000000000000000 ) ) ;
#3686 = EDGE_LOOP ( 'NONE', ( #7969, #12358, #14648, #14494 ) ) ;
#3687 = CARTESIAN_POINT ( 'NONE',  ( -69.77438362644001302, 82.17411849586700612, -83.44847958357698303 ) ) ;
#3688 = DIRECTION ( 'NONE',  ( 0.000000000000000000, 0.000000000000000000, 1.000000000000000000 ) ) ;
#3689 = PRODUCT_CONTEXT ( 'NONE', #10906, 'mechanical' ) ;
#3690 = ORIENTED_EDGE ( 'NONE', *, *, #12494, .F. ) ;
#3691 = AXIS2_PLACEMENT_3D ( 'NONE', #12765, #3294, #13629 ) ;
#3692 = CARTESIAN_POINT ( 'NONE',  ( 0.000000000000000000, 0.000000000000000000, 6.000000000000000000 ) ) ;
#3693 = CARTESIAN_POINT ( 'NONE',  ( -2.115018882620673057, -4.343749999999819700, -3.167137413913937660 ) ) ;
#3694 = VERTEX_POINT ( 'NONE', #5548 ) ;
#3695 = CARTESIAN_POINT ( 'NONE',  ( -1.113040416940756172, -1.288124999999980425, 3.674042195187707360 ) ) ;
#3696 = CARTESIAN_POINT ( 'NONE',  ( -15.50000000000000000, -0.4000000000000000222, 22.50000000000000000 ) ) ;
#3697 = DIRECTION ( 'NONE',  ( -0.000000000000000000, 1.000000000000000000, -0.000000000000000000 ) ) ;
#3698 = DIRECTION ( 'NONE',  ( 0.000000000000000000, 0.000000000000000000, -1.000000000000000000 ) ) ;
#3699 = FACE_BOUND ( 'NONE', #831, .T. ) ;
#3700 = DIRECTION ( 'NONE',  ( 0.000000000000000000, 0.000000000000000000, -1.000000000000000000 ) ) ;
#3701 = FACE_BOUND ( 'NONE', #836, .T. ) ;
#3702 = VERTEX_POINT ( 'NONE', #13476 ) ;
#3703 = LINE ( 'NONE', #8281, #9001 ) ;
#3704 = ADVANCED_FACE ( 'NONE', ( #6644 ), #14719, .T. ) ;
#3705 = ORIENTED_EDGE ( 'NONE', *, *, #430, .T. ) ;
#3706 = VERTEX_POINT ( 'NONE', #7867 ) ;
#3707 = CARTESIAN_POINT ( 'NONE',  ( 1.656526992905777762, -3.756875000000012399, -3.097233728230821548 ) ) ;
#3708 = VERTEX_POINT ( 'NONE', #13759 ) ;
#3709 = ORIENTED_EDGE ( 'NONE', *, *, #706, .F. ) ;
#3710 = ORIENTED_EDGE ( 'NONE', *, *, #319, .F. ) ;
#3711 = DIRECTION ( 'NONE',  ( 0.000000000000000000, 1.000000000000000000, 0.000000000000000000 ) ) ;
#3712 = CARTESIAN_POINT ( 'NONE',  ( -61.72438362644000165, 82.17411849586700612, -80.14847958357698587 ) ) ;
#3713 = CARTESIAN_POINT ( 'NONE',  ( -60.43728955831367955, 68.38713492810558137, -83.44847958357698303 ) ) ;
#3714 = PLANE ( 'NONE',  #10859 ) ;
#3715 = CARTESIAN_POINT ( 'NONE',  ( -86.77438362643999881, 67.53201699523744139, -147.9984795835769944 ) ) ;
#3716 = FACE_BOUND ( 'NONE', #10938, .T. ) ;
#3717 = ADVANCED_FACE ( 'NONE', ( #14901 ), #11021, .T. ) ;
#3718 = CARTESIAN_POINT ( 'NONE',  ( -3.406603204915101379, -4.053749999999936016, -0.6763000812039869913 ) ) ;
#3719 = DIRECTION ( 'NONE',  ( 0.000000000000000000, 0.000000000000000000, 1.000000000000000000 ) ) ;
#3720 = ORIENTED_EDGE ( 'NONE', *, *, #10881, .F. ) ;
#3721 = DIRECTION ( 'NONE',  ( -6.982962677686266711E-15, -6.579622859988665673E-30, -1.000000000000000000 ) ) ;
#3722 = EDGE_CURVE ( 'NONE', #11099, #1313, #3133, .T. ) ;
#3723 = EDGE_LOOP ( 'NONE', ( #13337, #34, #12304 ) ) ;
#3724 = EDGE_LOOP ( 'NONE', ( #12199, #13746, #6746, #13199 ) ) ;
#3725 = ORIENTED_EDGE ( 'NONE', *, *, #8959, .F. ) ;
#3726 = ORIENTED_EDGE ( 'NONE', *, *, #10777, .T. ) ;
#3727 = CARTESIAN_POINT ( 'NONE',  ( -15.50000000000000000, -0.4000000000005236034, 19.20000000000052509 ) ) ;
#3728 = CARTESIAN_POINT ( 'NONE',  ( -1.990045403832418236, -3.241250000000046594, 2.976654046991286329 ) ) ;
#3729 = LINE ( 'NONE', #8689, #2644 ) ;
#3730 = DIRECTION ( 'NONE',  ( -0.8660254037844482555, 0.000000000000000000, -0.4999999999999831801 ) ) ;
#3731 = FACE_BOUND ( 'NONE', #10209, .T. ) ;
#3732 = CARTESIAN_POINT ( 'NONE',  ( 1.403561989263862998E-14, -5.500000000000001776, 0.000000000000000000 ) ) ;
#3733 = FACE_OUTER_BOUND ( 'NONE', #6976, .T. ) ;
#3734 = DIRECTION ( 'NONE',  ( 0.000000000000000000, 0.000000000000000000, -1.000000000000000000 ) ) ;
#3735 = LINE ( 'NONE', #9625, #5096 ) ;
#3736 = EDGE_CURVE ( 'NONE', #1497, #913, #7565, .T. ) ;
#3737 = LINE ( 'NONE', #8467, #8569 ) ;
#3738 = CARTESIAN_POINT ( 'NONE',  ( -86.77438362644001302, 114.1741184958670061, -15.85886927678779834 ) ) ;
#3739 = ORIENTED_EDGE ( 'NONE', *, *, #805, .T. ) ;
#3740 = FACE_OUTER_BOUND ( 'NONE', #9188, .T. ) ;
#3741 = EDGE_CURVE ( 'NONE', #8134, #3619, #7010, .T. ) ;
#3742 = ORIENTED_EDGE ( 'NONE', *, *, #15169, .F. ) ;
#3743 = AXIS2_PLACEMENT_3D ( 'NONE', #11085, #457, #13492 ) ;
#3744 = ADVANCED_FACE ( 'NONE', ( #1418, #2344 ), #11887, .T. ) ;
#3745 = ORIENTED_EDGE ( 'NONE', *, *, #15097, .T. ) ;
#3746 = ORIENTED_EDGE ( 'NONE', *, *, #13059, .T. ) ;
#3747 = CARTESIAN_POINT ( 'NONE',  ( -16.75000000000000355, -0.2715193793361450614, -22.98718409945082541 ) ) ;
#3748 = CARTESIAN_POINT ( 'NONE',  ( 3.633142546501945791, -0.09374999999992907063, -2.429478397922130384 ) ) ;
#3749 = CARTESIAN_POINT ( 'NONE',  ( 4.232830310009522812, -0.9835885623730800109, 0.4180357722217523109 ) ) ;
#3750 = TOROIDAL_SURFACE ( 'NONE', #5493, 2.400000000000000355, 0.6000000000000000888 ) ;
#3751 = EDGE_CURVE ( 'NONE', #8660, #6308, #7094, .T. ) ;
#3752 = CYLINDRICAL_SURFACE ( 'NONE', #1635, 4.000000000000000000 ) ;
#3753 = DIRECTION ( 'NONE',  ( 1.287488025362404182E-15, 1.000000000000000000, 0.000000000000000000 ) ) ;
#3754 = CARTESIAN_POINT ( 'NONE',  ( -52.77438362644000591, 65.17411849586700612, -145.4984795835769660 ) ) ;
#3755 = VECTOR ( 'NONE', #5636, 1000.000000000000000 ) ;
#3756 = LINE ( 'NONE', #13230, #11003 ) ;
#3757 = EDGE_CURVE ( 'NONE', #13652, #4260, #3735, .T. ) ;
#3758 = DIRECTION ( 'NONE',  ( -1.000000000000000000, -0.000000000000000000, -0.000000000000000000 ) ) ;
#3759 = ORIENTED_EDGE ( 'NONE', *, *, #10451, .T. ) ;
#3760 = DIRECTION ( 'NONE',  ( 0.000000000000000000, 0.000000000000000000, 1.000000000000000000 ) ) ;
#3761 = EDGE_CURVE ( 'NONE', #2932, #3473, #2849, .T. ) ;
#3762 = CIRCLE ( 'NONE', #14153, 0.9999999999999991118 ) ;
#3763 = EDGE_CURVE ( 'NONE', #14989, #3401, #14972, .T. ) ;
#3764 = ORIENTED_EDGE ( 'NONE', *, *, #8205, .F. ) ;
#3765 = SURFACE_STYLE_USAGE ( .BOTH. , #8573 ) ;
#3766 = CARTESIAN_POINT ( 'NONE',  ( -3.756875241620029282, -3.453125000000005773, -1.140712293363390861 ) ) ;
#3767 = ORIENTED_EDGE ( 'NONE', *, *, #10977, .F. ) ;
#3768 = AXIS2_PLACEMENT_3D ( 'NONE', #9585, #8659, #14323 ) ;
#3769 =( REPRESENTATION_RELATIONSHIP ('NONE','NONE', #13541, #5010 ) REPRESENTATION_RELATIONSHIP_WITH_TRANSFORMATION ( #4936 )SHAPE_REPRESENTATION_RELATIONSHIP( ) );
#3770 = CARTESIAN_POINT ( 'NONE',  ( 0.3809421545653356445, -0.8193749999999933031, -3.882302026224086156 ) ) ;
#3771 = CARTESIAN_POINT ( 'NONE',  ( -77.52077156573416516, 164.3482369917340122, -79.59847958357700293 ) ) ;
#3772 = CIRCLE ( 'NONE', #43, 8.124999999999992895 ) ;
#3773 = DIRECTION ( 'NONE',  ( 8.034405899049458729E-17, 0.7547095802227716810, -0.6560590289905077199 ) ) ;
#3774 = AXIS2_PLACEMENT_3D ( 'NONE', #5256, #7441, #6284 ) ;
#3775 = DIRECTION ( 'NONE',  ( 0.000000000000000000, 0.000000000000000000, 1.000000000000000000 ) ) ;
#3776 = DIRECTION ( 'NONE',  ( 1.000000000000000000, 0.000000000000000000, 0.000000000000000000 ) ) ;
#3777 = LINE ( 'NONE', #1452, #8329 ) ;
#3778 = PLANE ( 'NONE',  #3139 ) ;
#3779 = ORIENTED_EDGE ( 'NONE', *, *, #14086, .T. ) ;
#3780 = DIRECTION ( 'NONE',  ( 0.000000000000000000, 0.000000000000000000, -1.000000000000000000 ) ) ;
#3781 = CARTESIAN_POINT ( 'NONE',  ( 7.616276556103071194, 41.51006470759390510, 188.8222949588812583 ) ) ;
#3782 = ORIENTED_EDGE ( 'NONE', *, *, #14908, .T. ) ;
#3783 = CARTESIAN_POINT ( 'NONE',  ( 2.598076211353308462, 2.375000000000006661, -4.499999999999999112 ) ) ;
#3784 = CARTESIAN_POINT ( 'NONE',  ( -3.184718056276182097, -3.006875000000130083, -1.703323619722392435 ) ) ;
#3785 = EDGE_LOOP ( 'NONE', ( #10845, #13823 ) ) ;
#3786 = ORIENTED_EDGE ( 'NONE', *, *, #7761, .T. ) ;
#3787 = VERTEX_POINT ( 'NONE', #8466 ) ;
#3788 = VECTOR ( 'NONE', #7067, 1000.000000000000000 ) ;
#3789 = DIRECTION ( 'NONE',  ( -0.000000000000000000, -0.000000000000000000, 1.000000000000000000 ) ) ;
#3790 = CARTESIAN_POINT ( 'NONE',  ( -3.471269930600009879, -5.271387000335979955, -0.1844037060100978398 ) ) ;
#3791 = DIRECTION ( 'NONE',  ( 0.000000000000000000, 0.000000000000000000, 1.000000000000000000 ) ) ;
#3792 = VECTOR ( 'NONE', #3432, 1000.000000000000000 ) ;
#3793 = CARTESIAN_POINT ( 'NONE',  ( -44.58670980944423690, 0.000000000000000000, 137.5095611191910621 ) ) ;
#3794 = DIRECTION ( 'NONE',  ( 0.000000000000000000, 0.000000000000000000, 1.000000000000000000 ) ) ;
#3795 = CARTESIAN_POINT ( 'NONE',  ( -14.24999999999999822, -0.2715193793361436736, -22.01281590054916038 ) ) ;
#3796 = CARTESIAN_POINT ( 'NONE',  ( 1.974738715674944078, -3.428749999999933795, 2.957050713271639708 ) ) ;
#3797 = DIRECTION ( 'NONE',  ( 1.000000000000000000, 0.000000000000000000, 0.000000000000000000 ) ) ;
#3798 = VERTEX_POINT ( 'NONE', #1180 ) ;
#3799 = DIRECTION ( 'NONE',  ( -1.000000000000000000, 0.000000000000000000, 0.000000000000000000 ) ) ;
#3800 = AXIS2_PLACEMENT_3D ( 'NONE', #2358, #12912, #7111 ) ;
#3801 = CIRCLE ( 'NONE', #6544, 0.8000000000000052625 ) ;
#3802 = ORIENTED_EDGE ( 'NONE', *, *, #2703, .F. ) ;
#3803 = ORIENTED_EDGE ( 'NONE', *, *, #14520, .T. ) ;
#3804 = ORIENTED_EDGE ( 'NONE', *, *, #7928, .T. ) ;
#3805 = ORIENTED_EDGE ( 'NONE', *, *, #4215, .T. ) ;
#3806 = AXIS2_PLACEMENT_3D ( 'NONE', #11178, #5300, #10015 ) ;
#3807 = LINE ( 'NONE', #2646, #6803 ) ;
#3808 = ADVANCED_FACE ( 'NONE', ( #7168 ), #5938, .F. ) ;
#3809 = CARTESIAN_POINT ( 'NONE',  ( -2.013335231365204425, -2.928749999999985310, -3.010762893885847280 ) ) ;
#3810 = DIRECTION ( 'NONE',  ( -1.000000000000000000, 0.000000000000000000, 0.000000000000000000 ) ) ;
#3811 = CARTESIAN_POINT ( 'NONE',  ( 3.056473733825995964, -5.095046775857358767, -2.078780392433921431 ) ) ;
#3812 = AXIS2_PLACEMENT_3D ( 'NONE', #5401, #6561, #13835 ) ;
#3813 = FACE_OUTER_BOUND ( 'NONE', #7190, .T. ) ;
#3814 = EDGE_CURVE ( 'NONE', #14332, #8449, #14063, .T. ) ;
#3815 = AXIS2_PLACEMENT_3D ( 'NONE', #2074, #4645, #9363 ) ;
#3816 = CARTESIAN_POINT ( 'NONE',  ( 2.598076211353315124, 0.1227504548087477720, 4.500000000000000000 ) ) ;
#3817 = DIRECTION ( 'NONE',  ( -0.000000000000000000, -0.000000000000000000, 1.000000000000000000 ) ) ;
#3818 = CARTESIAN_POINT ( 'NONE',  ( -69.77438362644001302, 82.17411849586700612, -44.99847958358509459 ) ) ;
#3819 = CARTESIAN_POINT ( 'NONE',  ( 17.18107410701653137, 3.665822296182962958, 0.1743669014992922095 ) ) ;
#3820 = CARTESIAN_POINT ( 'NONE',  ( 1.403561989263863629E-14, -5.500000000000003553, 0.000000000000000000 ) ) ;
#3821 = CARTESIAN_POINT ( 'NONE',  ( -15.50000000000000000, -1.037157890325000054, 22.50000000000000000 ) ) ;
#3822 = VERTEX_POINT ( 'NONE', #7239 ) ;
#3823 = PLANE ( 'NONE',  #13802 ) ;
#3824 = ORIENTED_EDGE ( 'NONE', *, *, #13061, .T. ) ;
#3825 = VERTEX_POINT ( 'NONE', #9468 ) ;
#3826 = ORIENTED_EDGE ( 'NONE', *, *, #7188, .T. ) ;
#3827 = CARTESIAN_POINT ( 'NONE',  ( -3.268702447147801227, -5.116250000000009734, 0.6493246907703037474 ) ) ;
#3828 = AXIS2_PLACEMENT_3D ( 'NONE', #9746, #4954, #9590 ) ;
#3829 = AXIS2_PLACEMENT_3D ( 'NONE', #8438, #13184, #13035 ) ;
#3830 = VECTOR ( 'NONE', #288, 1000.000000000000000 ) ;
#3831 = CARTESIAN_POINT ( 'NONE',  ( 4.294990272561590494, -0.03125000000009103135, -0.8531314740103178584 ) ) ;
#3832 = EDGE_CURVE ( 'NONE', #9574, #8280, #13069, .T. ) ;
#3833 = CARTESIAN_POINT ( 'NONE',  ( 1.994349568762445069, -1.171088562373031827, -3.728778841834516022 ) ) ;
#3834 = CARTESIAN_POINT ( 'NONE',  ( 22.58164641901421632, -12.00000029085423137, -56.77834603255778489 ) ) ;
#3835 = CARTESIAN_POINT ( 'NONE',  ( -101.2743836264399988, 114.1741184958669777, -67.49847958357700861 ) ) ;
#3836 = ADVANCED_FACE ( 'NONE', ( #13211 ), #10719, .F. ) ;
#3837 = DIRECTION ( 'NONE',  ( 0.000000000000000000, 0.000000000000000000, 1.000000000000000000 ) ) ;
#3838 = DIRECTION ( 'NONE',  ( 0.8660254037844482555, 0.000000000000000000, 0.4999999999999831801 ) ) ;
#3839 = VECTOR ( 'NONE', #8398, 1000.000000000000114 ) ;
#3840 = CARTESIAN_POINT ( 'NONE',  ( -69.77438362644001302, 82.17411849586700612, -81.84847958357698872 ) ) ;
#3841 = EDGE_LOOP ( 'NONE', ( #14195, #8684, #5909, #5050 ) ) ;
#3842 = DIRECTION ( 'NONE',  ( 0.000000000000000000, 0.000000000000000000, 1.000000000000000000 ) ) ;
#3843 = EDGE_CURVE ( 'NONE', #9156, #1855, #7319, .T. ) ;
#3844 = EDGE_CURVE ( 'NONE', #13430, #6768, #13762, .T. ) ;
#3845 = ITEM_DEFINED_TRANSFORMATION ( 'NONE', 'NONE', #3518,  #285 ) ;
#3846 = EDGE_LOOP ( 'NONE', ( #11493, #11515, #9934, #2047, #8092 ) ) ;
#3847 = CARTESIAN_POINT ( 'NONE',  ( -2.497846391779839248, -3.359374999999932943, -3.045264817802638468 ) ) ;
#3848 = EDGE_LOOP ( 'NONE', ( #8410, #15043, #12445, #609 ) ) ;
#3849 = EDGE_CURVE ( 'NONE', #1190, #14746, #10032, .T. ) ;
#3850 = CARTESIAN_POINT ( 'NONE',  ( 2.458139144364205109, -3.858588562373032271, 2.993019814648903765 ) ) ;
#3851 = VECTOR ( 'NONE', #843, 1000.000000000000000 ) ;
#3852 = CARTESIAN_POINT ( 'NONE',  ( 1.843713500184339216, -0.7568749999999383471, -3.447171040406491027 ) ) ;
#3853 = ADVANCED_FACE ( 'NONE', ( #12896 ), #2261, .T. ) ;
#3854 = CARTESIAN_POINT ( 'NONE',  ( 22.28931995216796835, -12.00000029085427222, 69.13384072020834026 ) ) ;
#3855 = ADVANCED_FACE ( 'NONE', ( #15288 ), #5063, .F. ) ;
#3856 = CYLINDRICAL_SURFACE ( 'NONE', #13705, 2.500000000000002220 ) ;
#3857 = FACE_OUTER_BOUND ( 'NONE', #12807, .T. ) ;
#3858 = LINE ( 'NONE', #8587, #8401 ) ;
#3859 = CARTESIAN_POINT ( 'NONE',  ( -30.00000000000000000, -5.000000000000000000, -43.00000000000002132 ) ) ;
#3860 = DIRECTION ( 'NONE',  ( 0.000000000000000000, 0.000000000000000000, 1.000000000000000000 ) ) ;
#3861 = DIRECTION ( 'NONE',  ( 0.000000000000000000, 0.000000000000000000, -1.000000000000000000 ) ) ;
#3862 =( GEOMETRIC_REPRESENTATION_CONTEXT ( 3 ) GLOBAL_UNCERTAINTY_ASSIGNED_CONTEXT ( ( #6702 ) ) GLOBAL_UNIT_ASSIGNED_CONTEXT ( ( #6237, #8616, #11022 ) ) REPRESENTATION_CONTEXT ( 'NONE', 'WORKASPACE' ) );
#3863 = ORIENTED_EDGE ( 'NONE', *, *, #2198, .F. ) ;
#3864 = CIRCLE ( 'NONE', #6363, 4.000000000000004441 ) ;
#3865 = CARTESIAN_POINT ( 'NONE',  ( -69.77438362644100778, 72.17411849586700612, -67.49847958357700861 ) ) ;
#3866 = ORIENTED_EDGE ( 'NONE', *, *, #2627, .T. ) ;
#3867 = ADVANCED_BREP_SHAPE_REPRESENTATION ( '', ( #330, #298, #5426, #10531, #10636, #285 ), #14401 ) ;
#3868 = DIRECTION ( 'NONE',  ( -1.000000000000000000, 0.000000000000000000, 6.860497997771530774E-15 ) ) ;
#3869 = CARTESIAN_POINT ( 'NONE',  ( 0.3573659033054734091, -2.819374999999921805, -3.618812876704415871 ) ) ;
#3870 = ORIENTED_EDGE ( 'NONE', *, *, #526, .F. ) ;
#3871 = VERTEX_POINT ( 'NONE', #1644 ) ;
#3872 = EDGE_CURVE ( 'NONE', #704, #9228, #9696, .T. ) ;
#3873 = CIRCLE ( 'NONE', #5613, 3.968749999999992895 ) ;
#3874 = AXIS2_PLACEMENT_3D ( 'NONE', #3373, #13849, #11441 ) ;
#3875 = DIRECTION ( 'NONE',  ( 0.000000000000000000, 1.000000000000000000, 0.000000000000000000 ) ) ;
#3876 = DIRECTION ( 'NONE',  ( 0.000000000000000000, 0.000000000000000000, -1.000000000000000000 ) ) ;
#3877 = CARTESIAN_POINT ( 'NONE',  ( 2.822529449220563258, -0.4995676945082517251, -2.935231339109197091 ) ) ;
#3878 = CARTESIAN_POINT ( 'NONE',  ( -69.77438362644001302, 82.17411849586700612, -67.69567958357700377 ) ) ;
#3879 = DIRECTION ( 'NONE',  ( 0.000000000000000000, 0.000000000000000000, -1.000000000000000000 ) ) ;
#3880 = EDGE_LOOP ( 'NONE', ( #12020, #11164, #135 ) ) ;
#3881 = CARTESIAN_POINT ( 'NONE',  ( -13.41835358098578723, -12.00000029085423670, -11.73358795631400930 ) ) ;
#3882 = VECTOR ( 'NONE', #4392, 1000.000000000000114 ) ;
#3883 = ORIENTED_EDGE ( 'NONE', *, *, #8478, .T. ) ;
#3884 = VECTOR ( 'NONE', #9163, 1000.000000000000000 ) ;
#3885 = ORIENTED_EDGE ( 'NONE', *, *, #10881, .T. ) ;
#3886 = EDGE_LOOP ( 'NONE', ( #7390, #11373, #12242, #6872, #174 ) ) ;
#3887 = ORIENTED_EDGE ( 'NONE', *, *, #6800, .T. ) ;
#3888 = LINE ( 'NONE', #1483, #6565 ) ;
#3889 = CARTESIAN_POINT ( 'NONE',  ( 2.926652851519762955, -1.694375000000067022, -2.400566300852225776 ) ) ;
#3890 = AXIS2_PLACEMENT_3D ( 'NONE', #12685, #890, #2058 ) ;
#3891 = CARTESIAN_POINT ( 'NONE',  ( -3.269128917323805172, -3.406249999999943601, -2.185603562728522853 ) ) ;
#3892 = FACE_BOUND ( 'NONE', #13411, .T. ) ;
#3893 = CARTESIAN_POINT ( 'NONE',  ( 7.511572993685698521E-16, 1.916901515185129432E-30, 4.500000000000000888 ) ) ;
#3894 = CIRCLE ( 'NONE', #12806, 2.750000000000002665 ) ;
#3895 = DIRECTION ( 'NONE',  ( 0.000000000000000000, 0.000000000000000000, -1.000000000000000000 ) ) ;
#3896 = CYLINDRICAL_SURFACE ( 'NONE', #6814, 3.000000000000002665 ) ;
#3897 = DIRECTION ( 'NONE',  ( -1.000000000000000000, 0.000000000000000000, 0.000000000000000000 ) ) ;
#3898 = CARTESIAN_POINT ( 'NONE',  ( -55.27438362644100067, 99.17411849586700612, -79.59847958357700293 ) ) ;
#3899 = DIRECTION ( 'NONE',  ( 0.000000000000000000, 1.000000000000000000, 0.000000000000000000 ) ) ;
#3900 = ORIENTED_EDGE ( 'NONE', *, *, #5844, .T. ) ;
#3901 = CARTESIAN_POINT ( 'NONE',  ( 16.59097840410232294, -11.89175346992432658, 0.2558260301694363359 ) ) ;
#3902 = VERTEX_POINT ( 'NONE', #14741 ) ;
#3903 = ORIENTED_EDGE ( 'NONE', *, *, #4317, .T. ) ;
#3904 = UNCERTAINTY_MEASURE_WITH_UNIT (LENGTH_MEASURE( 1.000000000000000082E-05 ), #13130, 'distance_accuracy_value', 'NONE');
#3905 = EDGE_CURVE ( 'NONE', #9134, #7307, #7819, .T. ) ;
#3906 = VECTOR ( 'NONE', #10971, 1000.000000000000114 ) ;
#3907 = DIRECTION ( 'NONE',  ( 0.000000000000000000, 0.000000000000000000, 1.000000000000000000 ) ) ;
#3908 = CARTESIAN_POINT ( 'NONE',  ( -3.186695398571379290, -5.131874999999967990, 0.9679749472946410638 ) ) ;
#3909 = LINE ( 'NONE', #3834, #6850 ) ;
#3910 = CARTESIAN_POINT ( 'NONE',  ( 21.98164641901421135, 11.99999970914576330, -14.13358795631400611 ) ) ;
#3911 = CARTESIAN_POINT ( 'NONE',  ( 16.99691247867024657, 3.654316742536408924, 0.2664120436859911956 ) ) ;
#3912 = CARTESIAN_POINT ( 'NONE',  ( 6.573385150445030689, -3.618985300545107364, 0.000000000000000000 ) ) ;
#3913 = CIRCLE ( 'NONE', #2922, 4.499999999999997335 ) ;
#3914 = CARTESIAN_POINT ( 'NONE',  ( 22.58164641901421632, -12.00000029085423670, -11.73358795631400930 ) ) ;
#3915 = ORIENTED_EDGE ( 'NONE', *, *, #9240, .T. ) ;
#3916 = CARTESIAN_POINT ( 'NONE',  ( -86.77438362644001302, 65.17411849586700612, -86.49847958357699440 ) ) ;
#3917 = EDGE_CURVE ( 'NONE', #8050, #7763, #2603, .T. ) ;
#3918 = CONTEXT_DEPENDENT_SHAPE_REPRESENTATION ( #11790, #5881 ) ;
#3919 = VERTEX_POINT ( 'NONE', #9857 ) ;
#3920 = CARTESIAN_POINT ( 'NONE',  ( 22.58164641901421277, -3.779330867977713115, -28.96834603255778262 ) ) ;
#3921 = CARTESIAN_POINT ( 'NONE',  ( 1.514604053328734823, -3.187500000000060396, -3.660349086209866876 ) ) ;
#3922 = ORIENTED_EDGE ( 'NONE', *, *, #9993, .T. ) ;
#3923 = CARTESIAN_POINT ( 'NONE',  ( -2.392265219297526002, -4.639838562373030051, 2.913436905822091028 ) ) ;
#3924 = AXIS2_PLACEMENT_3D ( 'NONE', #6916, #10148, #14879 ) ;
#3925 = CARTESIAN_POINT ( 'NONE',  ( 3.359686712365983929, -1.506874999999983755, 1.796916873358819222 ) ) ;
#3926 = CARTESIAN_POINT ( 'NONE',  ( -84.73238362643999722, 65.17411849586700612, -147.9984795835769944 ) ) ;
#3927 = ADVANCED_FACE ( 'NONE', ( #9776 ), #11176, .T. ) ;
#3928 = CARTESIAN_POINT ( 'NONE',  ( -1.733498803496027252, 11.99999970914575975, 38.15869532822594579 ) ) ;
#3929 = CARTESIAN_POINT ( 'NONE',  ( -4.522482571421201136, -12.00000029085427222, 70.03692566716181034 ) ) ;
#3930 = CARTESIAN_POINT ( 'NONE',  ( -54.81638362644100226, 99.17411849586700612, -147.9984795835769944 ) ) ;
#3931 = CARTESIAN_POINT ( 'NONE',  ( 2.898929819200243063, -5.329854288497422488, 1.773108554050290442 ) ) ;
#3932 = DIRECTION ( 'NONE',  ( -1.000000000000000000, 0.000000000000000000, -0.000000000000000000 ) ) ;
#3933 = DIRECTION ( 'NONE',  ( 0.000000000000000000, 0.000000000000000000, 1.000000000000000000 ) ) ;
#3934 = ADVANCED_FACE ( 'NONE', ( #7401 ), #6319, .F. ) ;
#3935 = DIRECTION ( 'NONE',  ( 0.000000000000000000, 0.000000000000000000, 1.000000000000000000 ) ) ;
#3936 = AXIS2_PLACEMENT_3D ( 'NONE', #13170, #12005, #3465 ) ;
#3937 = ORIENTED_EDGE ( 'NONE', *, *, #12854, .T. ) ;
#3938 = VERTEX_POINT ( 'NONE', #481 ) ;
#3939 = VERTEX_POINT ( 'NONE', #6466 ) ;
#3940 = EDGE_CURVE ( 'NONE', #411, #856, #6208, .T. ) ;
#3941 = LINE ( 'NONE', #11223, #13737 ) ;
#3942 = EDGE_CURVE ( 'NONE', #7562, #8783, #10012, .T. ) ;
#3943 = CARTESIAN_POINT ( 'NONE',  ( -3.586083906644842223, -3.069375000000151399, -0.3518610084925551384 ) ) ;
#3944 = VERTEX_POINT ( 'NONE', #14664 ) ;
#3945 = VERTEX_POINT ( 'NONE', #10953 ) ;
#3946 = DIRECTION ( 'NONE',  ( 0.000000000000000000, 0.000000000000000000, -1.000000000000000000 ) ) ;
#3947 = EDGE_CURVE ( 'NONE', #6550, #8981, #6102, .T. ) ;
#3948 = CARTESIAN_POINT ( 'NONE',  ( -80.52077156573417938, 164.3482369917340122, -152.4984795835769944 ) ) ;
#3949 = FACE_OUTER_BOUND ( 'NONE', #8737, .T. ) ;
#3950 = CARTESIAN_POINT ( 'NONE',  ( 2.088010756335936691, -0.4995676945082540010, -3.523544157046685221 ) ) ;
#3951 = CARTESIAN_POINT ( 'NONE',  ( -54.81638362644100226, 97.99516924618178848, -147.9984795835769944 ) ) ;
#3952 = EDGE_CURVE ( 'NONE', #3619, #4969, #12272, .T. ) ;
#3953 = PLANE ( 'NONE',  #8788 ) ;
#3954 = EDGE_LOOP ( 'NONE', ( #12650, #12360, #10606, #10463, #14346 ) ) ;
#3955 = CARTESIAN_POINT ( 'NONE',  ( 15.91434062215688350, -0.3156604612129282894, -23.70415600323552852 ) ) ;
#3956 = ORIENTED_EDGE ( 'NONE', *, *, #136, .T. ) ;
#3957 = ORIENTED_EDGE ( 'NONE', *, *, #14074, .T. ) ;
#3958 = VERTEX_POINT ( 'NONE', #403 ) ;
#3959 = VERTEX_POINT ( 'NONE', #5216 ) ;
#3960 = ORIENTED_EDGE ( 'NONE', *, *, #3200, .T. ) ;
#3961 = LINE ( 'NONE', #1779, #2334 ) ;
#3962 = CARTESIAN_POINT ( 'NONE',  ( 3.503209385669602938, -1.647500000000019948, -1.450007420588620866 ) ) ;
#3963 = CARTESIAN_POINT ( 'NONE',  ( 1.804739227294467563, -4.171875000000069278, -3.379404665904198968 ) ) ;
#3964 = DIRECTION ( 'NONE',  ( 0.000000000000000000, 0.000000000000000000, 1.000000000000000000 ) ) ;
#3965 = FACE_OUTER_BOUND ( 'NONE', #10527, .T. ) ;
#3966 = CARTESIAN_POINT ( 'NONE',  ( -4.991962918341529054, 1.883037081658660572, -0.3536665959326726338 ) ) ;
#3967 = CARTESIAN_POINT ( 'NONE',  ( -73.64736697264332577, 89.17411849586700612, -44.99847958359595168 ) ) ;
#3968 = LINE ( 'NONE', #7475, #12266 ) ;
#3969 = CARTESIAN_POINT ( 'NONE',  ( -81.27438362643999881, 82.17411849586700612, -82.44847958357698303 ) ) ;
#3970 = FACE_OUTER_BOUND ( 'NONE', #7906, .T. ) ;
#3971 = ORIENTED_EDGE ( 'NONE', *, *, #8199, .F. ) ;
#3972 = LINE ( 'NONE', #6547, #15177 ) ;
#3973 = VERTEX_POINT ( 'NONE', #12354 ) ;
#3974 = VERTEX_POINT ( 'NONE', #311 ) ;
#3975 = VERTEX_POINT ( 'NONE', #551 ) ;
#3976 = CARTESIAN_POINT ( 'NONE',  ( 0.9404171202241153882, -5.788124999999990195, -3.104336352551608336 ) ) ;
#3977 = DIRECTION ( 'NONE',  ( 0.000000000000000000, 0.000000000000000000, 1.000000000000000000 ) ) ;
#3978 = CARTESIAN_POINT ( 'NONE',  ( -0.001216256839607751574, -5.834999999999983977, -3.237452472516329838 ) ) ;
#3979 = FACE_OUTER_BOUND ( 'NONE', #12692, .T. ) ;
#3980 = LINE ( 'NONE', #8709, #6738 ) ;
#3981 = DIRECTION ( 'NONE',  ( 1.000000000000000000, 0.000000000000000000, 0.000000000000000000 ) ) ;
#3982 = FACE_OUTER_BOUND ( 'NONE', #5983, .T. ) ;
#3983 = DIRECTION ( 'NONE',  ( 0.000000000000000000, 0.000000000000000000, 1.000000000000000000 ) ) ;
#3984 = EDGE_CURVE ( 'NONE', #5926, #7246, #240, .T. ) ;
#3985 = PLANE ( 'NONE',  #8699 ) ;
#3986 = VERTEX_POINT ( 'NONE', #2655 ) ;
#3987 = CARTESIAN_POINT ( 'NONE',  ( 3.803621785104590794E-17, 9.355654565435173708, 0.000000000000000000 ) ) ;
#3988 = ORIENTED_EDGE ( 'NONE', *, *, #10107, .T. ) ;
#3989 = CIRCLE ( 'NONE', #3011, 3.000000000000002665 ) ;
#3990 = CARTESIAN_POINT ( 'NONE',  ( -86.77438362643999881, 65.17411849586700612, -146.8195303338917768 ) ) ;
#3991 = CARTESIAN_POINT ( 'NONE',  ( -2.876356209513419415, -2.375000000000007994, -2.877876508394843658 ) ) ;
#3992 = ORIENTED_EDGE ( 'NONE', *, *, #8743, .T. ) ;
#3993 = CARTESIAN_POINT ( 'NONE',  ( -1.836186059027842044, -3.671088562373069131, 3.438281954767565374 ) ) ;
#3994 = AXIS2_PLACEMENT_3D ( 'NONE', #10126, #10281, #1918 ) ;
#3995 = CYLINDRICAL_SURFACE ( 'NONE', #4739, 4.499999999999997335 ) ;
#3996 = EDGE_CURVE ( 'NONE', #5763, #2643, #5297, .T. ) ;
#3997 = CARTESIAN_POINT ( 'NONE',  ( 9.531855622864829864E-16, 8.384405323238834029, 0.000000000000000000 ) ) ;
#3998 = CARTESIAN_POINT ( 'NONE',  ( 15.50000000000000000, -5.000000000000000000, 22.50000000000000000 ) ) ;
#3999 = DIRECTION ( 'NONE',  ( -1.000000000000000000, 0.000000000000000000, 0.000000000000000000 ) ) ;
#4000 = EDGE_CURVE ( 'NONE', #4411, #10656, #3968, .T. ) ;
#4001 = AXIS2_PLACEMENT_3D ( 'NONE', #960, #5713, #7944 ) ;
#4002 = DIRECTION ( 'NONE',  ( -1.000000000000000000, 0.000000000000000000, 0.000000000000000000 ) ) ;
#4003 = FACE_BOUND ( 'NONE', #9476, .T. ) ;
#4004 = LINE ( 'NONE', #12319, #13546 ) ;
#4005 = CARTESIAN_POINT ( 'NONE',  ( 11.02372356922131758, -11.00000029085428110, 69.09311688316492450 ) ) ;
#4006 = DIRECTION ( 'NONE',  ( 0.000000000000000000, 0.000000000000000000, -1.000000000000000000 ) ) ;
#4007 = CIRCLE ( 'NONE', #2507, 3.968749999999992895 ) ;
#4008 = ORIENTED_EDGE ( 'NONE', *, *, #10092, .T. ) ;
#4009 = AXIS2_PLACEMENT_3D ( 'NONE', #7813, #7886, #1686 ) ;
#4010 = EDGE_LOOP ( 'NONE', ( #5759, #11391, #7857, #3340 ) ) ;
#4011 = CARTESIAN_POINT ( 'NONE',  ( -50.07438362643999596, 65.17411849586700612, -145.2984795835770058 ) ) ;
#4012 = CARTESIAN_POINT ( 'NONE',  ( -1.090659875871101692, -1.881874999999897602, -3.598793876473022735 ) ) ;
#4013 = VERTEX_POINT ( 'NONE', #14432 ) ;
#4014 = AXIS2_PLACEMENT_3D ( 'NONE', #7163, #9690, #14426 ) ;
#4015 = DIRECTION ( 'NONE',  ( 0.000000000000000000, 1.000000000000000000, 0.000000000000000000 ) ) ;
#4016 = EDGE_CURVE ( 'NONE', #11859, #12491, #4844, .T. ) ;
#4017 = VECTOR ( 'NONE', #860, 1000.000000000000000 ) ;
#4018 = CARTESIAN_POINT ( 'NONE',  ( -86.77438362643999881, 65.17411849586700612, -145.2984795835770058 ) ) ;
#4019 = AXIS2_PLACEMENT_3D ( 'NONE', #5651, #2363, #3298 ) ;
#4020 = CARTESIAN_POINT ( 'NONE',  ( -86.77438362644100778, 99.17411849586700612, -145.2984795835770058 ) ) ;
#4021 = EDGE_CURVE ( 'NONE', #14870, #467, #9284, .T. ) ;
#4022 = CARTESIAN_POINT ( 'NONE',  ( -86.77438362644001302, 65.17411849586700612, -86.49847958357699440 ) ) ;
#4023 = SURFACE_SIDE_STYLE ('',( #11310 ) ) ;
#4024 = DIRECTION ( 'NONE',  ( -2.551930889570659960E-15, 1.000000000000000000, 0.000000000000000000 ) ) ;
#4025 = DIRECTION ( 'NONE',  ( 1.084202172485504434E-16, -1.000000000000000000, -0.000000000000000000 ) ) ;
#4026 = CIRCLE ( 'NONE', #7983, 1.785937500000001066 ) ;
#4027 = ORIENTED_EDGE ( 'NONE', *, *, #12466, .F. ) ;
#4028 = CARTESIAN_POINT ( 'NONE',  ( 14.05000000000000249, -0.2000000000000000111, -22.50000000000000000 ) ) ;
#4029 = ORIENTED_EDGE ( 'NONE', *, *, #10366, .F. ) ;
#4030 = AXIS2_PLACEMENT_3D ( 'NONE', #5798, #11450, #9183 ) ;
#4031 = ADVANCED_FACE ( 'NONE', ( #12586, #8066, #1945, #13663, #4202 ), #9220, .F. ) ;
#4032 = ORIENTED_EDGE ( 'NONE', *, *, #137, .T. ) ;
#4033 = ORIENTED_EDGE ( 'NONE', *, *, #2509, .F. ) ;
#4034 = VERTEX_POINT ( 'NONE', #10150 ) ;
#4035 = VECTOR ( 'NONE', #355, 1000.000000000000000 ) ;
#4036 = ORIENTED_EDGE ( 'NONE', *, *, #11866, .T. ) ;
#4037 = DIRECTION ( 'NONE',  ( 0.000000000000000000, 0.000000000000000000, 1.000000000000000000 ) ) ;
#4038 = CARTESIAN_POINT ( 'NONE',  ( -3.566427039428707868, -2.131875000000089670, 1.083295335393480219 ) ) ;
#4039 = ADVANCED_FACE ( 'NONE', ( #3113 ), #6693, .T. ) ;
#4040 = VECTOR ( 'NONE', #1451, 1000.000000000000000 ) ;
#4041 = DIRECTION ( 'NONE',  ( 0.000000000000000000, 1.000000000000000000, 0.000000000000000000 ) ) ;
#4042 = CARTESIAN_POINT ( 'NONE',  ( -2.784563489868539410, -3.375000000000053735, -2.782533402055042071 ) ) ;
#4043 = CARTESIAN_POINT ( 'NONE',  ( -35.58670980944424400, 5.000000000000000000, 127.7236236191910734 ) ) ;
#4044 = CARTESIAN_POINT ( 'NONE',  ( 1.732658076282644233, 0.04645217140506596037, 4.500000000000000000 ) ) ;
#4045 = ADVANCED_FACE ( 'NONE', ( #11564 ), #15040, .T. ) ;
#4046 = EDGE_CURVE ( 'NONE', #15273, #13375, #14735, .T. ) ;
#4047 = CARTESIAN_POINT ( 'NONE',  ( -3.008642795497751266, 2.054436331234726687, -3.788877816371842844 ) ) ;
#4048 = CARTESIAN_POINT ( 'NONE',  ( -3.998008487304611336, -1.546875000000091038, 1.214361949261595131 ) ) ;
#4049 = CARTESIAN_POINT ( 'NONE',  ( -2.598076211353320453, 2.374999999999993339, 4.500000000000000888 ) ) ;
#4050 = AXIS2_PLACEMENT_3D ( 'NONE', #13698, #5716, #10186 ) ;
#4051 = CARTESIAN_POINT ( 'NONE',  ( -35.58670980944424400, 0.000000000000000000, 97.50956111919106206 ) ) ;
#4052 = VECTOR ( 'NONE', #13888, 1000.000000000000000 ) ;
#4053 = FACE_OUTER_BOUND ( 'NONE', #10055, .T. ) ;
#4054 = ORIENTED_EDGE ( 'NONE', *, *, #11063, .F. ) ;
#4055 = CARTESIAN_POINT ( 'NONE',  ( 10.10406781373725948, -11.00000029085427933, 69.08979243323352648 ) ) ;
#4056 = ORIENTED_EDGE ( 'NONE', *, *, #292, .T. ) ;
#4057 = AXIS2_PLACEMENT_3D ( 'NONE', #6322, #5066, #483 ) ;
#4058 = ORIENTED_EDGE ( 'NONE', *, *, #9979, .F. ) ;
#4059 = ORIENTED_EDGE ( 'NONE', *, *, #10132, .F. ) ;
#4060 = PRODUCT_DEFINITION_CONTEXT ( 'detailed design', #4867, 'design' ) ;
#4061 = FACE_OUTER_BOUND ( 'NONE', #14888, .T. ) ;
#4062 = VECTOR ( 'NONE', #2111, 1000.000000000000227 ) ;
#4063 = CARTESIAN_POINT ( 'NONE',  ( -86.77438362643999881, 65.17411849586700612, -149.9984795835770228 ) ) ;
#4064 = DIRECTION ( 'NONE',  ( -1.000000000000000000, 0.000000000000000000, 0.000000000000000000 ) ) ;
#4065 = DIRECTION ( 'NONE',  ( 0.000000000000000000, 0.000000000000000000, -1.000000000000000000 ) ) ;
#4066 = TOROIDAL_SURFACE ( 'NONE', #2823, 2.700000000000000178, 0.2000000000000000111 ) ;
#4067 = CARTESIAN_POINT ( 'NONE',  ( -88.81638362644100937, 99.17411849586700612, -147.9984795835769944 ) ) ;
#4068 = CARTESIAN_POINT ( 'NONE',  ( 1.916065064279496746E-15, 7.362499999999997158, 0.000000000000000000 ) ) ;
#4069 = APPLICATION_CONTEXT ( 'automotive_design' ) ;
#4070 = DIRECTION ( 'NONE',  ( -0.000000000000000000, -0.000000000000000000, -1.000000000000000000 ) ) ;
#4071 = ORIENTED_EDGE ( 'NONE', *, *, #9703, .T. ) ;
#4072 = CARTESIAN_POINT ( 'NONE',  ( -52.77438362644100067, 101.5320169952374414, -150.4984795835770228 ) ) ;
#4073 = AXIS2_PLACEMENT_3D ( 'NONE', #4727, #7214, #4891 ) ;
#4074 = CIRCLE ( 'NONE', #1591, 2.000000000000001776 ) ;
#4075 = ITEM_DEFINED_TRANSFORMATION ( 'NONE', 'NONE', #4030,  #1538 ) ;
#4076 = EDGE_LOOP ( 'NONE', ( #12161, #7975, #10642, #15115 ) ) ;
#4077 = CARTESIAN_POINT ( 'NONE',  ( -1.898222722261231343, -2.671874999999975131, 3.554431989243950873 ) ) ;
#4078 = ORIENTED_EDGE ( 'NONE', *, *, #14917, .T. ) ;
#4079 = VECTOR ( 'NONE', #6507, 1000.000000000000000 ) ;
#4080 = CARTESIAN_POINT ( 'NONE',  ( -96.77438362643999881, 65.17411849586700612, -152.4984795835769944 ) ) ;
#4081 = AXIS2_PLACEMENT_3D ( 'NONE', #12408, #603, #1993 ) ;
#4082 = CARTESIAN_POINT ( 'NONE',  ( -13.16982544356192797, -12.00000029085424025, 0.01788390626213304940 ) ) ;
#4083 = CARTESIAN_POINT ( 'NONE',  ( -3.127990687458618524, 2.260916199238038718E-16, 54.09781049769389227 ) ) ;
#4084 = DIRECTION ( 'NONE',  ( 0.000000000000000000, 0.000000000000000000, 1.000000000000000000 ) ) ;
#4085 = DIRECTION ( 'NONE',  ( 0.000000000000000000, 0.000000000000000000, -1.000000000000000000 ) ) ;
#4086 = DIRECTION ( 'NONE',  ( -1.000000000000000000, 0.000000000000000000, 0.000000000000000000 ) ) ;
#4087 = FACE_BOUND ( 'NONE', #8202, .T. ) ;
#4088 = DIRECTION ( 'NONE',  ( 0.000000000000000000, 0.000000000000000000, -1.000000000000000000 ) ) ;
#4089 = ORIENTED_EDGE ( 'NONE', *, *, #5193, .F. ) ;
#4090 = EDGE_CURVE ( 'NONE', #13263, #6604, #851, .T. ) ;
#4091 =( NAMED_UNIT ( * ) SI_UNIT ( $, .STERADIAN. ) SOLID_ANGLE_UNIT ( ) );
#4092 = ORIENTED_EDGE ( 'NONE', *, *, #11601, .F. ) ;
#4093 = CARTESIAN_POINT ( 'NONE',  ( -69.77438362644001302, 74.17411849586699191, -58.99847958357700151 ) ) ;
#4094 = CARTESIAN_POINT ( 'NONE',  ( 2.926652851519856213, -1.694375000000067022, -2.400566300852225776 ) ) ;
#4095 = VERTEX_POINT ( 'NONE', #7985 ) ;
#4096 = AXIS2_PLACEMENT_3D ( 'NONE', #4598, #3431, #8165 ) ;
#4097 = EDGE_CURVE ( 'NONE', #5891, #8137, #6841, .T. ) ;
#4098 = DIRECTION ( 'NONE',  ( -1.000000000000000000, 0.000000000000000000, 0.000000000000000000 ) ) ;
#4099 = PRODUCT_DEFINITION_SHAPE ( 'NONE', 'NONE',  #10143 ) ;
#4100 = CARTESIAN_POINT ( 'NONE',  ( 1.453141968011759877, -5.138246789499178568, -3.363386372659848966 ) ) ;
#4101 = LINE ( 'NONE', #14790, #2076 ) ;
#4102 = CIRCLE ( 'NONE', #12770, 17.00000000000000000 ) ;
#4103 = CARTESIAN_POINT ( 'NONE',  ( 0.3070149676124478977, -0.4995676945082583309, -4.130607965512141710 ) ) ;
#4104 = DIRECTION ( 'NONE',  ( 0.000000000000000000, 1.000000000000000000, 0.000000000000000000 ) ) ;
#4105 = AXIS2_PLACEMENT_3D ( 'NONE', #12170, #13420, #12105 ) ;
#4106 = CARTESIAN_POINT ( 'NONE',  ( -1.733498803496028140, -12.00000029085427578, 38.15869532822594579 ) ) ;
#4107 = DIRECTION ( 'NONE',  ( 1.060575238724893480E-16, 0.5000000000000189848, -0.8660254037844277164 ) ) ;
#4108 = ORIENTED_EDGE ( 'NONE', *, *, #980, .T. ) ;
#4109 = LINE ( 'NONE', #4187, #6794 ) ;
#4110 = EDGE_CURVE ( 'NONE', #2784, #13871, #768, .T. ) ;
#4111 = EDGE_CURVE ( 'NONE', #5237, #3237, #4498, .T. ) ;
#4112 = ORIENTED_EDGE ( 'NONE', *, *, #15156, .T. ) ;
#4113 = EDGE_LOOP ( 'NONE', ( #4321, #8157, #13567, #14612, #6699 ) ) ;
#4114 = VERTEX_POINT ( 'NONE', #701 ) ;
#4115 = AXIS2_PLACEMENT_3D ( 'NONE', #8325, #2491, #14361 ) ;
#4116 = ORIENTED_EDGE ( 'NONE', *, *, #2131, .T. ) ;
#4117 = ORIENTED_EDGE ( 'NONE', *, *, #10758, .T. ) ;
#4118 = AXIS2_PLACEMENT_3D ( 'NONE', #11830, #13228, #15304 ) ;
#4119 = CARTESIAN_POINT ( 'NONE',  ( -89.52438362644001302, 99.17411849586700612, -145.4984795835769660 ) ) ;
#4120 = AXIS2_PLACEMENT_3D ( 'NONE', #2926, #7736, #4086 ) ;
#4121 = CARTESIAN_POINT ( 'NONE',  ( 3.730555813499059070, -1.553749999999926246, 0.7430650243616524486 ) ) ;
#4122 = CARTESIAN_POINT ( 'NONE',  ( -3.331846864947428877, -4.578125000000028422, 1.779793940175935729 ) ) ;
#4123 = DIRECTION ( 'NONE',  ( -0.000000000000000000, -0.000000000000000000, 1.000000000000000000 ) ) ;
#4124 = EDGE_CURVE ( 'NONE', #11097, #840, #11260, .T. ) ;
#4125 = DIRECTION ( 'NONE',  ( -1.000000000000000000, 0.000000000000000000, 0.000000000000000000 ) ) ;
#4126 = CARTESIAN_POINT ( 'NONE',  ( -3.490494984142799684, -1.406250000000081268, -2.330449509171077516 ) ) ;
#4127 = EDGE_CURVE ( 'NONE', #2251, #4356, #5588, .T. ) ;
#4128 = CONICAL_SURFACE ( 'NONE', #8824, 3.968749999999992895, 0.7155849933176756661 ) ;
#4129 = CARTESIAN_POINT ( 'NONE',  ( -54.81638362644000040, 63.99516924618178848, -147.9984795835769944 ) ) ;
#4130 = DIRECTION ( 'NONE',  ( -1.287488025362404182E-15, -1.000000000000000000, 0.000000000000000000 ) ) ;
#4131 = CARTESIAN_POINT ( 'NONE',  ( 40.52020888806953991, 0.000000000000000000, 6.000000000000000000 ) ) ;
#4132 = AXIS2_PLACEMENT_3D ( 'NONE', #14128, #14507, #12044 ) ;
#4133 = ORIENTED_EDGE ( 'NONE', *, *, #13793, .T. ) ;
#4134 = AXIS2_PLACEMENT_3D ( 'NONE', #10025, #3047, #5463 ) ;
#4135 = DIRECTION ( 'NONE',  ( 0.000000000000000000, 0.000000000000000000, 1.000000000000000000 ) ) ;
#4136 = EDGE_CURVE ( 'NONE', #5494, #14030, #12722, .T. ) ;
#4137 = EDGE_LOOP ( 'NONE', ( #3726, #13114, #9782, #10790, #10405 ) ) ;
#4138 = ORIENTED_EDGE ( 'NONE', *, *, #3257, .T. ) ;
#4139 = ORIENTED_EDGE ( 'NONE', *, *, #4376, .T. ) ;
#4140 = EDGE_CURVE ( 'NONE', #469, #840, #12647, .T. ) ;
#4141 = LINE ( 'NONE', #11272, #5502 ) ;
#4142 = EDGE_CURVE ( 'NONE', #587, #11316, #3344, .T. ) ;
#4143 = VECTOR ( 'NONE', #5794, 1000.000000000000000 ) ;
#4144 = CARTESIAN_POINT ( 'NONE',  ( -1.520556115814812870, -5.913125000000218456, -2.846480943363819183 ) ) ;
#4145 = AXIS2_PLACEMENT_3D ( 'NONE', #12879, #15105, #5831 ) ;
#4146 = DIRECTION ( 'NONE',  ( 1.000000000000000000, 0.000000000000000000, 0.000000000000000000 ) ) ;
#4147 = DIRECTION ( 'NONE',  ( 0.000000000000000000, -4.130293990420970006E-17, 1.000000000000000000 ) ) ;
#4148 = CARTESIAN_POINT ( 'NONE',  ( 14.25000000000000000, -0.2038245569916330158, -23.22168783648699986 ) ) ;
#4149 = EDGE_CURVE ( 'NONE', #14022, #263, #1862, .T. ) ;
#4150 = CARTESIAN_POINT ( 'NONE',  ( -80.27438362643999881, 82.17411849586700612, -82.44847958357698303 ) ) ;
#4151 = CARTESIAN_POINT ( 'NONE',  ( -73.03793661009240168, 75.17411849586699191, -44.70344037800862225 ) ) ;
#4152 = CARTESIAN_POINT ( 'NONE',  ( 1.903042727507366250, -4.428749999999965326, 2.845810502761935368 ) ) ;
#4153 = EDGE_LOOP ( 'NONE', ( #13314, #1852, #1423, #11744 ) ) ;
#4154 = VECTOR ( 'NONE', #1024, 1000.000000000000000 ) ;
#4155 = DIRECTION ( 'NONE',  ( 0.8660254037844383745, -0.5000000000000003331, 0.000000000000000000 ) ) ;
#4156 = EDGE_CURVE ( 'NONE', #3473, #2932, #5848, .T. ) ;
#4157 = VECTOR ( 'NONE', #13934, 1000.000000000000000 ) ;
#4158 = VERTEX_POINT ( 'NONE', #11484 ) ;
#4159 = CARTESIAN_POINT ( 'NONE',  ( 4.118464008547413790, -2.000000000000003109, 0.001090570402295849319 ) ) ;
#4160 = ORIENTED_EDGE ( 'NONE', *, *, #5326, .F. ) ;
#4161 = CARTESIAN_POINT ( 'NONE',  ( 1.125729777374074869, -3.796088562373163722, 3.714534500553497764 ) ) ;
#4162 = DIRECTION ( 'NONE',  ( 0.000000000000000000, 0.000000000000000000, -1.000000000000000000 ) ) ;
#4163 = DIRECTION ( 'NONE',  ( 0.000000000000000000, -0.000000000000000000, 1.000000000000000000 ) ) ;
#4164 = AXIS2_PLACEMENT_3D ( 'NONE', #82, #12982, #13137 ) ;
#4165 = CARTESIAN_POINT ( 'NONE',  ( -42.77438362644000591, 59.67411849586700612, -152.4984795835769944 ) ) ;
#4166 = CARTESIAN_POINT ( 'NONE',  ( -77.52077156573416516, 60.67411849586702743, -152.4984795835769944 ) ) ;
#4167 = CARTESIAN_POINT ( 'NONE',  ( 2.931404194366990623, 4.650702586819546624, 3.589934763638662607E-16 ) ) ;
#4168 = LINE ( 'NONE', #4314, #3132 ) ;
#4169 = CARTESIAN_POINT ( 'NONE',  ( -67.06350624369862601, 97.94473565475263399, -93.86023119279390414 ) ) ;
#4170 = DIRECTION ( 'NONE',  ( -0.000000000000000000, -0.000000000000000000, 1.000000000000000000 ) ) ;
#4171 = ORIENTED_EDGE ( 'NONE', *, *, #10051, .F. ) ;
#4172 = ORIENTED_EDGE ( 'NONE', *, *, #10258, .F. ) ;
#4173 = VECTOR ( 'NONE', #4661, 1000.000000000000000 ) ;
#4174 = DIRECTION ( 'NONE',  ( 1.000000000000000000, 0.000000000000000000, 0.000000000000000000 ) ) ;
#4175 = CARTESIAN_POINT ( 'NONE',  ( -0.7236788045118249801, -2.303749999999964437, 3.633254187536902879 ) ) ;
#4176 = VERTEX_POINT ( 'NONE', #9148 ) ;
#4177 = FACE_BOUND ( 'NONE', #11802, .T. ) ;
#4178 = CARTESIAN_POINT ( 'NONE',  ( -86.77438362643999881, 65.17411849586700612, -182.2484795835770228 ) ) ;
#4179 = DIRECTION ( 'NONE',  ( 0.8660254037844383745, -0.5000000000000003331, 0.000000000000000000 ) ) ;
#4180 = AXIS2_PLACEMENT_3D ( 'NONE', #4022, #8750, #377 ) ;
#4181 = CARTESIAN_POINT ( 'NONE',  ( -15.50000000000000000, 998.9628421096749662, -22.50000000000000000 ) ) ;
#4182 = DIRECTION ( 'NONE',  ( 0.4999999999999827360, 0.000000000000000000, 0.8660254037844485886 ) ) ;
#4183 = DIRECTION ( 'NONE',  ( 0.000000000000000000, 0.000000000000000000, 1.000000000000000000 ) ) ;
#4184 = EDGE_CURVE ( 'NONE', #11099, #9860, #7328, .T. ) ;
#4185 = CARTESIAN_POINT ( 'NONE',  ( -64.53565528768383786, 67.29799558322736175, -81.84847958357697451 ) ) ;
#4186 = EDGE_LOOP ( 'NONE', ( #7973, #3960, #7484, #2458 ) ) ;
#4187 = CARTESIAN_POINT ( 'NONE',  ( -85.77438362644001302, 82.17411849586700612, -183.7533135795160320 ) ) ;
#4188 = ORIENTED_EDGE ( 'NONE', *, *, #13109, .T. ) ;
#4189 = ORIENTED_EDGE ( 'NONE', *, *, #10652, .F. ) ;
#4190 = ORIENTED_EDGE ( 'NONE', *, *, #7354, .T. ) ;
#4191 = EDGE_LOOP ( 'NONE', ( #6328, #7079, #15276, #11995, #6286 ) ) ;
#4192 = EDGE_LOOP ( 'NONE', ( #1109, #1254, #3475, #8246 ) ) ;
#4193 = AXIS2_PLACEMENT_3D ( 'NONE', #2689, #5020, #11140 ) ;
#4194 = CARTESIAN_POINT ( 'NONE',  ( 3.570415799723221095, -6.014838562373082453, -0.3529878125807653366 ) ) ;
#4195 = LINE ( 'NONE', #1710, #2114 ) ;
#4196 = CARTESIAN_POINT ( 'NONE',  ( -3.756875241620029282, -3.453125000000005773, -1.140712293363390861 ) ) ;
#4197 = LINE ( 'NONE', #763, #13212 ) ;
#4198 = EDGE_CURVE ( 'NONE', #12948, #188, #14339, .T. ) ;
#4199 = CARTESIAN_POINT ( 'NONE',  ( -13.41835358098578723, -12.00000029085423670, -11.73358795631401463 ) ) ;
#4200 = DIRECTION ( 'NONE',  ( 0.000000000000000000, 0.000000000000000000, -1.000000000000000000 ) ) ;
#4201 = CARTESIAN_POINT ( 'NONE',  ( 4.172905853428635403, -0.9687499999999248379, 0.8311981373062848899 ) ) ;
#4202 = FACE_OUTER_BOUND ( 'NONE', #5744, .T. ) ;
#4203 = FACE_OUTER_BOUND ( 'NONE', #12173, .T. ) ;
#4204 = EDGE_CURVE ( 'NONE', #14751, #8552, #11023, .T. ) ;
#4205 = CARTESIAN_POINT ( 'NONE',  ( 16.75000000000000000, -0.2038245569916320166, 23.22168783648699986 ) ) ;
#4206 = ORIENTED_EDGE ( 'NONE', *, *, #1576, .T. ) ;
#4207 = CARTESIAN_POINT ( 'NONE',  ( -1.629699455448989389E-14, 8.699999999999999289, 5.655858585055787181E-29 ) ) ;
#4208 = ORIENTED_EDGE ( 'NONE', *, *, #3375, .T. ) ;
#4209 = ORIENTED_EDGE ( 'NONE', *, *, #10858, .F. ) ;
#4210 = VERTEX_POINT ( 'NONE', #4662 ) ;
#4211 = DIRECTION ( 'NONE',  ( 1.000000000000000000, 0.000000000000000000, 0.000000000000000000 ) ) ;
#4212 = CARTESIAN_POINT ( 'NONE',  ( -1.864549691619314498, -4.928749999999819664, -2.792029179168366237 ) ) ;
#4213 = LINE ( 'NONE', #6557, #8551 ) ;
#4214 = CARTESIAN_POINT ( 'NONE',  ( -73.80978675135780520, 64.78624853950366003, -81.84847958357697451 ) ) ;
#4215 = EDGE_CURVE ( 'NONE', #4974, #3454, #14042, .T. ) ;
#4216 = DIRECTION ( 'NONE',  ( -0.000000000000000000, -0.000000000000000000, -1.000000000000000000 ) ) ;
#4217 = CARTESIAN_POINT ( 'NONE',  ( -52.77438362644100067, 99.17411849586700612, -150.4984795835770228 ) ) ;
#4218 = CARTESIAN_POINT ( 'NONE',  ( 1.213339409441202221, -0.4995676945082561660, 3.847960304831221645 ) ) ;
#4219 = ADVANCED_FACE ( 'NONE', ( #10621, #8302, #3716, #13121, #11870, #14269 ), #3411, .F. ) ;
#4220 = FACE_OUTER_BOUND ( 'NONE', #13671, .T. ) ;
#4221 = EDGE_CURVE ( 'NONE', #6290, #1968, #9301, .T. ) ;
#4222 = VERTEX_POINT ( 'NONE', #14115 ) ;
#4223 = CARTESIAN_POINT ( 'NONE',  ( 15.08565937784311117, -0.3156604612129225162, 23.70415600323552852 ) ) ;
#4224 = ORIENTED_EDGE ( 'NONE', *, *, #1933, .F. ) ;
#4225 = DIRECTION ( 'NONE',  ( 0.000000000000000000, 0.000000000000000000, 1.000000000000000000 ) ) ;
#4226 = ORIENTED_EDGE ( 'NONE', *, *, #13577, .F. ) ;
#4227 = EDGE_CURVE ( 'NONE', #9170, #1220, #8301, .T. ) ;
#4228 = CARTESIAN_POINT ( 'NONE',  ( 1.536269025742735383, -2.812500000000037303, 3.705069426614713723 ) ) ;
#4229 = VERTEX_POINT ( 'NONE', #2241 ) ;
#4230 = LINE ( 'NONE', #5484, #7478 ) ;
#4231 = ADVANCED_FACE ( 'NONE', ( #6987 ), #7072, .F. ) ;
#4232 = DIRECTION ( 'NONE',  ( -0.000000000000000000, -0.000000000000000000, 1.000000000000000000 ) ) ;
#4233 = DIRECTION ( 'NONE',  ( 1.000000000000000000, 0.000000000000000000, 0.000000000000000000 ) ) ;
#4234 = ADVANCED_FACE ( 'NONE', ( #14187 ), #2471, .F. ) ;
#4235 = CARTESIAN_POINT ( 'NONE',  ( -13.41835358098578723, -12.00000029085423670, -14.13358795631400611 ) ) ;
#4236 = EDGE_CURVE ( 'NONE', #10374, #8857, #15188, .T. ) ;
#4237 = CARTESIAN_POINT ( 'NONE',  ( -2.598076211353319120, 1.678847577293364424, 4.500000000000000888 ) ) ;
#4238 = CARTESIAN_POINT ( 'NONE',  ( -3.897114317029974462, -9.945166405816860437E-15, 2.249999999999999112 ) ) ;
#4239 = FACE_BOUND ( 'NONE', #5153, .T. ) ;
#4240 = CARTESIAN_POINT ( 'NONE',  ( 16.75000000000000000, -2.500000000000000000, 23.22168783648699986 ) ) ;
#4241 = AXIS2_PLACEMENT_3D ( 'NONE', #1891, #11356, #1965 ) ;
#4242 = EDGE_LOOP ( 'NONE', ( #15234, #13528, #3120, #1949 ) ) ;
#4243 = CARTESIAN_POINT ( 'NONE',  ( 17.04394838817069768, -11.40000029085424238, 0.2824263826447100945 ) ) ;
#4244 = CARTESIAN_POINT ( 'NONE',  ( -0.3768771888558096750, -1.319375000000004405, 3.816279424444235513 ) ) ;
#4245 = ORIENTED_EDGE ( 'NONE', *, *, #9961, .F. ) ;
#4246 = CARTESIAN_POINT ( 'NONE',  ( -52.77438362644000591, 99.17411849586700612, -86.49847958357699440 ) ) ;
#4247 = AXIS2_PLACEMENT_3D ( 'NONE', #420, #5312, #4064 ) ;
#4248 = DIRECTION ( 'NONE',  ( 0.000000000000000000, 1.000000000000000000, 0.000000000000000000 ) ) ;
#4249 = AXIS2_PLACEMENT_3D ( 'NONE', #10575, #11898, #6104 ) ;
#4250 = CARTESIAN_POINT ( 'NONE',  ( 57.41329019055577021, 5.000000000000001776, 129.5095611191910621 ) ) ;
#4251 = CARTESIAN_POINT ( 'NONE',  ( -3.476613658449263955, 2.260916199238038718E-16, 58.08258929006087357 ) ) ;
#4252 = CARTESIAN_POINT ( 'NONE',  ( -62.02799568714584666, 59.67411849586701322, -79.59847958357700293 ) ) ;
#4253 = EDGE_LOOP ( 'NONE', ( #4484, #13637, #15096, #13890 ) ) ;
#4254 = CARTESIAN_POINT ( 'NONE',  ( -14.66434062215825840, -0.3156604612126666654, 23.46090750622624910 ) ) ;
#4255 = EDGE_LOOP ( 'NONE', ( #3674, #6935, #13180, #8209 ) ) ;
#4256 = AXIS2_PLACEMENT_3D ( 'NONE', #12801, #12961, #4732 ) ;
#4257 = ORIENTED_EDGE ( 'NONE', *, *, #4490, .T. ) ;
#4258 = ORIENTED_EDGE ( 'NONE', *, *, #6345, .T. ) ;
#4259 = ORIENTED_EDGE ( 'NONE', *, *, #8010, .T. ) ;
#4260 = VERTEX_POINT ( 'NONE', #3566 ) ;
#4261 = CARTESIAN_POINT ( 'NONE',  ( -3.263656433892394126, -6.436713562373405750, -1.350434304814589925 ) ) ;
#4262 = AXIS2_PLACEMENT_3D ( 'NONE', #2299, #7050, #10600 ) ;
#4263 = CARTESIAN_POINT ( 'NONE',  ( -1.834300037444539511, -0.9131249999999379030, -3.428720741157346374 ) ) ;
#4264 = CARTESIAN_POINT ( 'NONE',  ( 63.41329019055576310, 0.000000000000000000, 137.5095611191910621 ) ) ;
#4265 = CARTESIAN_POINT ( 'NONE',  ( 0.4056240317150583419, -1.765625000000045741, 4.129595427369183724 ) ) ;
#4266 = DIRECTION ( 'NONE',  ( -1.000000000000000000, 0.000000000000000000, 0.000000000000000000 ) ) ;
#4267 = FACE_OUTER_BOUND ( 'NONE', #4508, .T. ) ;
#4268 = VECTOR ( 'NONE', #14760, 1000.000000000000000 ) ;
#4269 = FACE_OUTER_BOUND ( 'NONE', #9008, .T. ) ;
#4270 = CARTESIAN_POINT ( 'NONE',  ( -69.77438362644001302, 90.17411849586700612, -58.99847958357700151 ) ) ;
#4271 = DIRECTION ( 'NONE',  ( -0.000000000000000000, 0.000000000000000000, 1.000000000000000000 ) ) ;
#4272 = DIRECTION ( 'NONE',  ( -0.000000000000000000, -0.000000000000000000, 1.000000000000000000 ) ) ;
#4273 = CARTESIAN_POINT ( 'NONE',  ( -16.75000000000000000, -0.2038245569916330158, -21.77831216351300014 ) ) ;
#4274 = PRODUCT_DEFINITION_FORMATION_WITH_SPECIFIED_SOURCE ( 'ANY', '', #9565, .NOT_KNOWN. ) ;
#4275 = VERTEX_POINT ( 'NONE', #5756 ) ;
#4276 = DIRECTION ( 'NONE',  ( 0.000000000000000000, 0.000000000000000000, 1.000000000000000000 ) ) ;
#4277 = VECTOR ( 'NONE', #6118, 1000.000000000000000 ) ;
#4278 = ORIENTED_EDGE ( 'NONE', *, *, #3660, .T. ) ;
#4279 = ORIENTED_EDGE ( 'NONE', *, *, #886, .F. ) ;
#4280 = ORIENTED_EDGE ( 'NONE', *, *, #7929, .F. ) ;
#4281 = EDGE_CURVE ( 'NONE', #3437, #9494, #9526, .T. ) ;
#4282 = AXIS2_PLACEMENT_3D ( 'NONE', #13864, #8198, #15245 ) ;
#4283 = PLANE ( 'NONE',  #10705 ) ;
#4284 = EDGE_CURVE ( 'NONE', #2501, #14624, #10540, .T. ) ;
#4285 = CARTESIAN_POINT ( 'NONE',  ( 16.99691247867024657, -3.654316742536411589, 0.2664120436859911956 ) ) ;
#4286 = DIRECTION ( 'NONE',  ( 0.000000000000000000, 1.000000000000000000, 0.000000000000000000 ) ) ;
#4287 = VECTOR ( 'NONE', #7981, 1000.000000000000000 ) ;
#4288 = AXIS2_PLACEMENT_3D ( 'NONE', #14192, #13126, #6078 ) ;
#4289 = DIRECTION ( 'NONE',  ( 0.000000000000000000, 0.000000000000000000, 1.000000000000000000 ) ) ;
#4290 = CARTESIAN_POINT ( 'NONE',  ( 2.919796888921922573, -5.104126807837104707, -2.256669152708658643 ) ) ;
#4291 = CARTESIAN_POINT ( 'NONE',  ( -71.44964421664379017, 75.17411849586702033, -44.18949531478482839 ) ) ;
#4292 = DIRECTION ( 'NONE',  ( 0.8660254037844482555, 0.000000000000000000, -0.4999999999999831801 ) ) ;
#4293 = CIRCLE ( 'NONE', #2300, 0.5000000000000000000 ) ;
#4294 = CARTESIAN_POINT ( 'NONE',  ( -3.090028468548657425, -5.022500000000056808, -1.280849571915205765 ) ) ;
#4295 = EDGE_LOOP ( 'NONE', ( #2176, #611, #11593, #6994 ) ) ;
#4296 = CARTESIAN_POINT ( 'NONE',  ( -86.77438362643999881, 67.53201699523744139, -147.9984795835769944 ) ) ;
#4297 = VERTEX_POINT ( 'NONE', #11943 ) ;
#4298 = EDGE_CURVE ( 'NONE', #14347, #7132, #13530, .T. ) ;
#4299 = ORIENTED_EDGE ( 'NONE', *, *, #14000, .F. ) ;
#4300 = VECTOR ( 'NONE', #2154, 999.9999999999998863 ) ;
#4301 = CARTESIAN_POINT ( 'NONE',  ( -3.324804228637022074, -0.6093749999999287237, 2.730601746129839746 ) ) ;
#4302 = ORIENTED_EDGE ( 'NONE', *, *, #3940, .T. ) ;
#4303 = ADVANCED_FACE ( 'NONE', ( #6071 ), #10784, .F. ) ;
#4304 = VECTOR ( 'NONE', #11262, 1000.000000000000114 ) ;
#4305 = FACE_OUTER_BOUND ( 'NONE', #14298, .T. ) ;
#4306 = DIRECTION ( 'NONE',  ( 0.000000000000000000, 0.000000000000000000, 1.000000000000000000 ) ) ;
#4307 = CARTESIAN_POINT ( 'NONE',  ( 15.50000000000000000, -0.4000000000005274892, 22.50000000000000000 ) ) ;
#4308 = AXIS2_PLACEMENT_3D ( 'NONE', #6783, #10330, #12442 ) ;
#4309 = VECTOR ( 'NONE', #11685, 1000.000000000000000 ) ;
#4310 = ADVANCED_FACE ( 'NONE', ( #15267 ), #9674, .T. ) ;
#4311 = FACE_OUTER_BOUND ( 'NONE', #2463, .T. ) ;
#4312 = FACE_OUTER_BOUND ( 'NONE', #6532, .T. ) ;
#4313 = EDGE_CURVE ( 'NONE', #8137, #1184, #3122, .T. ) ;
#4314 = CARTESIAN_POINT ( 'NONE',  ( -13.41835358098578723, 11.39999970914576366, -11.73358795631400397 ) ) ;
#4315 = CARTESIAN_POINT ( 'NONE',  ( -46.58670980944423690, 0.000000000000000000, 91.50956111919106206 ) ) ;
#4316 = CARTESIAN_POINT ( 'NONE',  ( 15.50000000000000000, -0.2000000000000000111, 22.50000000000000000 ) ) ;
#4317 = EDGE_CURVE ( 'NONE', #14576, #6162, #14492, .T. ) ;
#4318 = VERTEX_POINT ( 'NONE', #2709 ) ;
#4319 = CARTESIAN_POINT ( 'NONE',  ( -86.77438362644100778, 99.17411849586700612, -150.4984795835770228 ) ) ;
#4320 = CARTESIAN_POINT ( 'NONE',  ( 2.949251946438324889, -1.475624999999980647, 2.418581166398251714 ) ) ;
#4321 = ORIENTED_EDGE ( 'NONE', *, *, #12659, .F. ) ;
#4322 = VECTOR ( 'NONE', #10920, 1000.000000000000000 ) ;
#4323 = CONICAL_SURFACE ( 'NONE', #3316, 1732.050807568785558, 1.047197551196574761 ) ;
#4324 = AXIS2_PLACEMENT_3D ( 'NONE', #12227, #13101, #9581 ) ;
#4325 = ADVANCED_FACE ( 'NONE', ( #6448 ), #1131, .T. ) ;
#4326 = EDGE_CURVE ( 'NONE', #16, #9472, #12039, .T. ) ;
#4327 = DIRECTION ( 'NONE',  ( 0.000000000000000000, 0.000000000000000000, 1.000000000000000000 ) ) ;
#4328 = CARTESIAN_POINT ( 'NONE',  ( -50.73238362643999722, 65.17411849586700612, -147.9984795835769944 ) ) ;
#4329 = FACE_OUTER_BOUND ( 'NONE', #8432, .T. ) ;
#4330 = CARTESIAN_POINT ( 'NONE',  ( 2.573385150445055114, -19.31989681812820692, 6.000000000000001776 ) ) ;
#4331 = DIRECTION ( 'NONE',  ( 0.000000000000000000, 1.000000000000000000, 0.000000000000000000 ) ) ;
#4332 = DIRECTION ( 'NONE',  ( -1.000000000000000000, 0.000000000000000000, 0.000000000000000000 ) ) ;
#4333 = AXIS2_PLACEMENT_3D ( 'NONE', #14319, #3697, #2688 ) ;
#4334 = DIRECTION ( 'NONE',  ( 0.000000000000000000, 1.000000000000000000, 0.000000000000000000 ) ) ;
#4335 = ORIENTED_EDGE ( 'NONE', *, *, #9906, .F. ) ;
#4336 = AXIS2_PLACEMENT_3D ( 'NONE', #9378, #8381, #5919 ) ;
#4337 = DIRECTION ( 'NONE',  ( 0.000000000000000000, 0.000000000000000000, 1.000000000000000000 ) ) ;
#4338 = EDGE_CURVE ( 'NONE', #12409, #14932, #12333, .T. ) ;
#4339 = EDGE_LOOP ( 'NONE', ( #3476, #7874 ) ) ;
#4340 = VERTEX_POINT ( 'NONE', #291 ) ;
#4341 = CARTESIAN_POINT ( 'NONE',  ( 1.242853247313903786, -5.772499999999809006, -2.998378529913433788 ) ) ;
#4342 = ORIENTED_EDGE ( 'NONE', *, *, #14827, .F. ) ;
#4343 = EDGE_LOOP ( 'NONE', ( #12689, #15249, #4361, #12221, #1534 ) ) ;
#4344 = ORIENTED_EDGE ( 'NONE', *, *, #6304, .F. ) ;
#4345 = CARTESIAN_POINT ( 'NONE',  ( -0.7085372255082872384, -5.717963562373346242, 3.557256890250359849 ) ) ;
#4346 = CARTESIAN_POINT ( 'NONE',  ( -1.113040416940756172, -1.288124999999980425, 3.674042195187707360 ) ) ;
#4347 = VECTOR ( 'NONE', #8650, 1000.000000000000000 ) ;
#4348 = AXIS2_PLACEMENT_3D ( 'NONE', #12124, #6242, #6397 ) ;
#4349 = CARTESIAN_POINT ( 'NONE',  ( 3.968938162104017842, -2.984375000000153211, 0.3919611025626033030 ) ) ;
#4350 = DIRECTION ( 'NONE',  ( 1.000000000000000000, 0.000000000000000000, 0.000000000000000000 ) ) ;
#4351 = FACE_OUTER_BOUND ( 'NONE', #3672, .T. ) ;
#4352 = CARTESIAN_POINT ( 'NONE',  ( -53.70938362644000819, 81.46011849586699327, -81.84847958357697451 ) ) ;
#4353 = CARTESIAN_POINT ( 'NONE',  ( -47.27438362644100778, 57.67411849586700612, -79.49847958357700861 ) ) ;
#4354 = CARTESIAN_POINT ( 'NONE',  ( 35.35543536254876074, -19.31989681812820692, 6.000000000000001776 ) ) ;
#4355 = LINE ( 'NONE', #14817, #12222 ) ;
#4356 = VERTEX_POINT ( 'NONE', #9911 ) ;
#4357 = CARTESIAN_POINT ( 'NONE',  ( -69.77438362644001302, 82.17411849586700612, -3.496191900462991775 ) ) ;
#4358 = MECHANICAL_DESIGN_GEOMETRIC_PRESENTATION_REPRESENTATION (  '', ( #6609 ), #7592 ) ;
#4359 = ORIENTED_EDGE ( 'NONE', *, *, #11240, .F. ) ;
#4360 = ORIENTED_EDGE ( 'NONE', *, *, #3098, .F. ) ;
#4361 = ORIENTED_EDGE ( 'NONE', *, *, #2104, .T. ) ;
#4362 = AXIS2_PLACEMENT_3D ( 'NONE', #6917, #1310, #4576 ) ;
#4363 = CARTESIAN_POINT ( 'NONE',  ( -65.73898050152220662, 64.78624853950366003, -83.44847958357698303 ) ) ;
#4364 = CARTESIAN_POINT ( 'NONE',  ( 2.619799856955864925, -4.694374999999869402, -2.148899555557211904 ) ) ;
#4365 = DIRECTION ( 'NONE',  ( 1.000000000000000000, 0.000000000000000000, 0.000000000000000000 ) ) ;
#4366 = CIRCLE ( 'NONE', #3126, 1.785937500000001066 ) ;
#4367 = CARTESIAN_POINT ( 'NONE',  ( -69.77438362644002723, 75.17411849587348627, -43.99847958364158984 ) ) ;
#4368 = CYLINDRICAL_SURFACE ( 'NONE', #892, 16.00000000000000000 ) ;
#4369 = AXIS2_PLACEMENT_3D ( 'NONE', #12188, #13515, #13438 ) ;
#4370 = CARTESIAN_POINT ( 'NONE',  ( 15.50000000000000000, -0.2038245569916610489, -23.94337567297399971 ) ) ;
#4371 = CARTESIAN_POINT ( 'NONE',  ( 2.377331891390069174, -0.4995676945082533349, 3.200807742935684264 ) ) ;
#4372 = AXIS2_PLACEMENT_3D ( 'NONE', #6134, #11370, #1909 ) ;
#4373 = DIRECTION ( 'NONE',  ( 0.000000000000000000, 0.000000000000000000, -1.000000000000000000 ) ) ;
#4374 = ORIENTED_EDGE ( 'NONE', *, *, #10279, .T. ) ;
#4375 = CARTESIAN_POINT ( 'NONE',  ( -82.27438362643999881, 99.17411849586700612, -145.4984795835769660 ) ) ;
#4376 = EDGE_CURVE ( 'NONE', #2744, #4095, #1397, .T. ) ;
#4377 = ORIENTED_EDGE ( 'NONE', *, *, #9140, .F. ) ;
#4378 = CARTESIAN_POINT ( 'NONE',  ( -89.52438362644001302, 99.17411849586700612, -152.4984795835769944 ) ) ;
#4379 = VECTOR ( 'NONE', #8492, 1000.000000000000000 ) ;
#4380 = EDGE_LOOP ( 'NONE', ( #2157, #11248, #2155, #13077 ) ) ;
#4381 = CIRCLE ( 'NONE', #12316, 0.9999999999999991118 ) ;
#4382 = CARTESIAN_POINT ( 'NONE',  ( -1.962865815818235271, -1.671875000000012879, 3.669921287786785502 ) ) ;
#4383 = VERTEX_POINT ( 'NONE', #2551 ) ;
#4384 = CARTESIAN_POINT ( 'NONE',  ( 0.7848530992743523171, -2.780463562373096664, 3.938237677807348902 ) ) ;
#4385 = CARTESIAN_POINT ( 'NONE',  ( -3.127990687458618524, 2.260916199238038718E-16, 54.09781049769389227 ) ) ;
#4386 = PLANE ( 'NONE',  #8816 ) ;
#4387 = CARTESIAN_POINT ( 'NONE',  ( 22.58164641901421632, -11.40000029085423705, -11.73358795631401463 ) ) ;
#4388 = CIRCLE ( 'NONE', #6389, 4.000000000000000000 ) ;
#4389 = EDGE_CURVE ( 'NONE', #10402, #51, #13024, .T. ) ;
#4390 = AXIS2_PLACEMENT_3D ( 'NONE', #13757, #3051, #5467 ) ;
#4391 = FACE_OUTER_BOUND ( 'NONE', #8269, .T. ) ;
#4392 = DIRECTION ( 'NONE',  ( 0.8660254037844482555, 0.000000000000000000, -0.4999999999999831801 ) ) ;
#4393 = CARTESIAN_POINT ( 'NONE',  ( -1.673688575075004152E-15, 4.650702586819541295, 0.000000000000000000 ) ) ;
#4394 = ORIENTED_EDGE ( 'NONE', *, *, #14226, .F. ) ;
#4395 = FILL_AREA_STYLE_COLOUR ( '', #5843 ) ;
#4396 = CARTESIAN_POINT ( 'NONE',  ( -0.7729260235471412388, -0.3037499999998679590, 3.893172034236696444 ) ) ;
#4397 = ORIENTED_EDGE ( 'NONE', *, *, #3009, .F. ) ;
#4398 = VECTOR ( 'NONE', #9466, 1000.000000000000000 ) ;
#4399 = ADVANCED_FACE ( 'NONE', ( #531 ), #5354, .T. ) ;
#4400 = CARTESIAN_POINT ( 'NONE',  ( 1.779210140229128934, -1.756874999999983755, -3.331607052712222572 ) ) ;
#4401 = CARTESIAN_POINT ( 'NONE',  ( 17.18164641901421419, -2.908542394189813650E-07, 0.2664120436859911956 ) ) ;
#4402 = DIRECTION ( 'NONE',  ( 0.000000000000000000, 1.000000000000000000, 0.000000000000000000 ) ) ;
#4403 = EDGE_CURVE ( 'NONE', #4486, #2946, #12021, .T. ) ;
#4404 = LINE ( 'NONE', #5270, #4562 ) ;
#4405 = CARTESIAN_POINT ( 'NONE',  ( -69.77438362644001302, 82.17411849586700612, -43.99847958357699440 ) ) ;
#4406 = CARTESIAN_POINT ( 'NONE',  ( -69.77438362644001302, 82.17411849586700612, -29.37106258560738681 ) ) ;
#4407 = ADVANCED_FACE ( 'NONE', ( #14639 ), #9838, .F. ) ;
#4408 = CARTESIAN_POINT ( 'NONE',  ( 17.12895037488186389, 10.99999970914575620, 0.2687305842673423095 ) ) ;
#4409 = AXIS2_PLACEMENT_3D ( 'NONE', #2321, #9889, #4731 ) ;
#4410 = ADVANCED_FACE ( 'NONE', ( #13271 ), #8807, .T. ) ;
#4411 = VERTEX_POINT ( 'NONE', #380 ) ;
#4412 = CARTESIAN_POINT ( 'NONE',  ( -59.27438362644000591, 82.17411849586700612, -152.4984795835769944 ) ) ;
#4413 = VERTEX_POINT ( 'NONE', #8676 ) ;
#4414 = ORIENTED_EDGE ( 'NONE', *, *, #14450, .T. ) ;
#4415 = ORIENTED_EDGE ( 'NONE', *, *, #4127, .F. ) ;
#4416 = ORIENTED_EDGE ( 'NONE', *, *, #10666, .F. ) ;
#4417 = VERTEX_POINT ( 'NONE', #221 ) ;
#4418 = CARTESIAN_POINT ( 'NONE',  ( -89.27438362644100778, 110.1741184958670061, -79.59847958357700293 ) ) ;
#4419 = EDGE_CURVE ( 'NONE', #8823, #8783, #463, .T. ) ;
#4420 = CARTESIAN_POINT ( 'NONE',  ( 3.756292859848789689, -0.6318749999998841682, -1.140955529460117690 ) ) ;
#4421 = CONICAL_SURFACE ( 'NONE', #15059, 3.968749999999992895, 0.7155849933176756661 ) ;
#4422 = SURFACE_STYLE_FILL_AREA ( #6756 ) ;
#4423 = CARTESIAN_POINT ( 'NONE',  ( 3.414669715040141273, -2.093749999999965805, -2.280302418758094252 ) ) ;
#4424 = DIRECTION ( 'NONE',  ( 1.000000000000000000, 0.000000000000000000, 0.000000000000000000 ) ) ;
#4425 = ADVANCED_FACE ( 'NONE', ( #2780 ), #10931, .T. ) ;
#4426 = CARTESIAN_POINT ( 'NONE',  ( -69.77438362644001302, 81.46011849586699327, -83.44847958357698303 ) ) ;
#4427 = CARTESIAN_POINT ( 'NONE',  ( 4.991962918341520172, 1.883037081658684775, 0.3536665959326708575 ) ) ;
#4428 = LINE ( 'NONE', #12721, #8719 ) ;
#4429 = CARTESIAN_POINT ( 'NONE',  ( -52.77438362643999881, 67.53201699523744139, -147.9984795835769944 ) ) ;
#4430 = LINE ( 'NONE', #7987, #14522 ) ;
#4431 = CARTESIAN_POINT ( 'NONE',  ( -80.27438362643999881, 82.17411849586700612, -150.4984795835769944 ) ) ;
#4432 = EDGE_LOOP ( 'NONE', ( #1361, #10020, #4224, #14251 ) ) ;
#4433 = CARTESIAN_POINT ( 'NONE',  ( -14.66242688423474227, -0.3152598339554795182, -23.45980260912095616 ) ) ;
#4434 = EDGE_LOOP ( 'NONE', ( #4861, #10356, #11362, #11266 ) ) ;
#4435 = AXIS2_PLACEMENT_3D ( 'NONE', #14697, #12085, #4084 ) ;
#4436 = VERTEX_POINT ( 'NONE', #7533 ) ;
#4437 = ORIENTED_EDGE ( 'NONE', *, *, #2625, .T. ) ;
#4438 = FACE_OUTER_BOUND ( 'NONE', #4380, .T. ) ;
#4439 = CARTESIAN_POINT ( 'NONE',  ( 0.6686498792469546260, -4.366249999999815223, 3.366016213005436075 ) ) ;
#4440 = B_SPLINE_CURVE_WITH_KNOTS ( 'NONE', 3,
 ( #9120, #3227, #13859, #2216 ),
 .UNSPECIFIED., .F., .F.,
 ( 4, 4 ),
 ( 0.004347030683767774163, 0.006950528372497996078 ),
 .UNSPECIFIED. ) ;
#4441 = CARTESIAN_POINT ( 'NONE',  ( -77.89938362643999881, 82.17411849586700612, -79.49847958357700861 ) ) ;
#4442 = DIRECTION ( 'NONE',  ( -0.000000000000000000, 1.000000000000000000, 4.336808689942017736E-16 ) ) ;
#4443 = CARTESIAN_POINT ( 'NONE',  ( -6.060835862730317059E-15, 2.375000000000000000, 0.000000000000000000 ) ) ;
#4444 = CARTESIAN_POINT ( 'NONE',  ( -69.77438362644001302, 82.17411849586700612, -93.49847958357699440 ) ) ;
#4445 = CARTESIAN_POINT ( 'NONE',  ( -15.50000000000000000, -2.500000000000000000, -23.94337567297399971 ) ) ;
#4446 = CARTESIAN_POINT ( 'NONE',  ( -2.028590488616179410, -0.4995676945082638820, 3.621854581741517531 ) ) ;
#4447 = DIRECTION ( 'NONE',  ( 1.000000000000000000, 0.000000000000000000, 0.000000000000000000 ) ) ;
#4448 = SHAPE_REPRESENTATION ( 'Self-Tapping Grease Fitting_8742T12', ( #285 ), #8480 ) ;
#4449 = ORIENTED_EDGE ( 'NONE', *, *, #11979, .T. ) ;
#4450 = DIRECTION ( 'NONE',  ( -0.000000000000000000, -1.000000000000000000, -0.000000000000000000 ) ) ;
#4451 = ORIENTED_EDGE ( 'NONE', *, *, #13613, .T. ) ;
#4452 = EDGE_LOOP ( 'NONE', ( #5783, #1480, #11630, #6291 ) ) ;
#4453 = LINE ( 'NONE', #14909, #12167 ) ;
#4454 = VERTEX_POINT ( 'NONE', #10363 ) ;
#4455 = CARTESIAN_POINT ( 'NONE',  ( -3.980019242547642833, -0.5625000000000109912, 1.650257999534034514 ) ) ;
#4456 = ORIENTED_EDGE ( 'NONE', *, *, #7343, .T. ) ;
#4457 = CARTESIAN_POINT ( 'NONE',  ( 3.798302739331970379, -2.061713562373112651, -1.572130684568777692 ) ) ;
#4458 = CARTESIAN_POINT ( 'NONE',  ( -15.50000000000000000, -5.000000000000000000, -22.50000000000000000 ) ) ;
#4459 = ADVANCED_FACE ( 'NONE', ( #2071 ), #15017, .T. ) ;
#4460 = CARTESIAN_POINT ( 'NONE',  ( -69.77438362644001302, 81.46011849586699327, -83.44847958357698303 ) ) ;
#4461 = DIRECTION ( 'NONE',  ( -0.7071067811865474617, 8.659560562354921765E-17, 0.7071067811865474617 ) ) ;
#4462 = FACE_OUTER_BOUND ( 'NONE', #556, .T. ) ;
#4463 = CARTESIAN_POINT ( 'NONE',  ( 3.250000000000017764, 7.362500000000000711, 0.000000000000000000 ) ) ;
#4464 = PLANE ( 'NONE',  #7255 ) ;
#4465 = ORIENTED_EDGE ( 'NONE', *, *, #6320, .F. ) ;
#4466 = SURFACE_STYLE_USAGE ( .BOTH. , #10274 ) ;
#4467 = CARTESIAN_POINT ( 'NONE',  ( 3.430119610663647567, -5.062500000000104805, -1.422280051980938431 ) ) ;
#4468 = ORIENTED_EDGE ( 'NONE', *, *, #3335, .T. ) ;
#4469 = ADVANCED_FACE ( 'NONE', ( #3014 ), #9127, .F. ) ;
#4470 = CARTESIAN_POINT ( 'NONE',  ( 3.601230736643932673, -2.553749999999958220, 0.7149504581460995878 ) ) ;
#4471 = DIRECTION ( 'NONE',  ( -0.000000000000000000, -1.000000000000000000, -0.000000000000000000 ) ) ;
#4472 = EDGE_CURVE ( 'NONE', #5280, #6026, #9055, .T. ) ;
#4473 = CARTESIAN_POINT ( 'NONE',  ( 57.41329019055577021, 2.488961461112888074, 131.2954986191910791 ) ) ;
#4474 = CARTESIAN_POINT ( 'NONE',  ( -15.50000000000000000, -0.2000000000000000111, 25.79999999999947136 ) ) ;
#4475 = LINE ( 'NONE', #979, #8074 ) ;
#4476 = CARTESIAN_POINT ( 'NONE',  ( -69.77438362644001302, 82.17411849586700612, -81.84847958357698872 ) ) ;
#4477 = CONICAL_SURFACE ( 'NONE', #13417, 4.500000000000000888, 1.396263401595466691 ) ;
#4478 = ORIENTED_EDGE ( 'NONE', *, *, #9056, .F. ) ;
#4479 = DIRECTION ( 'NONE',  ( 0.000000000000000000, 0.000000000000000000, -1.000000000000000000 ) ) ;
#4480 = VERTEX_POINT ( 'NONE', #14793 ) ;
#4481 = ORIENTED_EDGE ( 'NONE', *, *, #8959, .T. ) ;
#4482 = CARTESIAN_POINT ( 'NONE',  ( 0.9808155824294417791, -4.788124999999903153, -3.230360883553722307 ) ) ;
#4483 = ORIENTED_EDGE ( 'NONE', *, *, #6703, .F. ) ;
#4484 = ORIENTED_EDGE ( 'NONE', *, *, #12812, .F. ) ;
#4485 = EDGE_CURVE ( 'NONE', #5494, #3511, #7756, .T. ) ;
#4486 = VERTEX_POINT ( 'NONE', #1844 ) ;
#4487 = AXIS2_PLACEMENT_3D ( 'NONE', #12311, #9960, #1901 ) ;
#4488 = CARTESIAN_POINT ( 'NONE',  ( -1.671015529475609052, -6.327338562373312492, -3.128183168801260461 ) ) ;
#4489 = CARTESIAN_POINT ( 'NONE',  ( -1.153796164589722117, -0.2881249999999724309, 3.799958344797442766 ) ) ;
#4490 = EDGE_CURVE ( 'NONE', #8420, #2616, #8565, .T. ) ;
#4491 = AXIS2_PLACEMENT_3D ( 'NONE', #8934, #2666, #8865 ) ;
#4492 = DIRECTION ( 'NONE',  ( 0.000000000000000000, 0.000000000000000000, -1.000000000000000000 ) ) ;
#4493 = CARTESIAN_POINT ( 'NONE',  ( 1.953452353076893244, -1.828124999999917399, 3.651470988527475647 ) ) ;
#4494 = DIRECTION ( 'NONE',  ( 0.000000000000000000, 0.000000000000000000, -1.000000000000000000 ) ) ;
#4495 = CARTESIAN_POINT ( 'NONE',  ( -52.77438362643999881, 67.53201699523744139, -150.4984795835770228 ) ) ;
#4496 = CARTESIAN_POINT ( 'NONE',  ( 3.440513747128896682, 2.288586792248404223, 3.040855385833559854 ) ) ;
#4497 = DIRECTION ( 'NONE',  ( -9.422394424380278809E-16, 1.000000000000000000, -0.000000000000000000 ) ) ;
#4498 = LINE ( 'NONE', #2012, #8798 ) ;
#4499 = DIRECTION ( 'NONE',  ( 0.000000000000000000, 0.000000000000000000, -1.000000000000000000 ) ) ;
#4500 = CARTESIAN_POINT ( 'NONE',  ( -53.77438362644000591, 82.17411849586700612, -93.49847958357699440 ) ) ;
#4501 = VECTOR ( 'NONE', #23, 1000.000000000000000 ) ;
#4502 = EDGE_CURVE ( 'NONE', #11163, #3634, #9348, .T. ) ;
#4503 = VERTEX_POINT ( 'NONE', #4251 ) ;
#4504 = EDGE_CURVE ( 'NONE', #14951, #7919, #11381, .T. ) ;
#4505 = CARTESIAN_POINT ( 'NONE',  ( 1.581646419014213878, 11.39999970914575655, 0.2664120436859911956 ) ) ;
#4506 = VERTEX_POINT ( 'NONE', #3089 ) ;
#4507 = EDGE_LOOP ( 'NONE', ( #14904, #10335, #3639, #11947 ) ) ;
#4508 = EDGE_LOOP ( 'NONE', ( #4644, #13507, #1677, #13032 ) ) ;
#4509 = VECTOR ( 'NONE', #5813, 1000.000000000000000 ) ;
#4510 = ADVANCED_FACE ( 'NONE', ( #907 ), #7827, .F. ) ;
#4511 = CARTESIAN_POINT ( 'NONE',  ( -83.02438362644100778, 99.17411849586700612, -150.4984795835770228 ) ) ;
#4512 = CARTESIAN_POINT ( 'NONE',  ( -3.406603204915101379, -4.053749999999936016, -0.6763000812039869913 ) ) ;
#4513 = EDGE_CURVE ( 'NONE', #8072, #6629, #10206, .T. ) ;
#4514 = CIRCLE ( 'NONE', #6511, 1.999999999999988010 ) ;
#4515 = EDGE_CURVE ( 'NONE', #5656, #1184, #14752, .T. ) ;
#4516 = DIRECTION ( 'NONE',  ( 0.8660254037844383745, -0.5000000000000003331, 0.000000000000000000 ) ) ;
#4517 = CARTESIAN_POINT ( 'NONE',  ( -68.42626121176353138, 75.17411849586696349, -44.11946707556869995 ) ) ;
#4518 = CARTESIAN_POINT ( 'NONE',  ( -0.4546285099643554983, 2.357490090282483131, -4.499999999999999112 ) ) ;
#4519 = CARTESIAN_POINT ( 'NONE',  ( -52.77438362643999881, 65.17411849586700612, -79.59847958357700293 ) ) ;
#4520 = DIRECTION ( 'NONE',  ( 0.000000000000000000, 0.000000000000000000, -1.000000000000000000 ) ) ;
#4521 = LINE ( 'NONE', #3503, #10742 ) ;
#4522 = CARTESIAN_POINT ( 'NONE',  ( -15.50000000000000000, -2.500000000000000000, -21.05662432702600029 ) ) ;
#4523 = AXIS2_PLACEMENT_3D ( 'NONE', #3452, #4542, #7032 ) ;
#4524 = ORIENTED_EDGE ( 'NONE', *, *, #8948, .F. ) ;
#4525 = DIRECTION ( 'NONE',  ( 1.000000000000000000, 0.000000000000000000, 0.000000000000000000 ) ) ;
#4526 = ORIENTED_EDGE ( 'NONE', *, *, #8285, .T. ) ;
#4527 = STYLED_ITEM ( 'NONE', ( #4715 ), #10716 ) ;
#4528 = ORIENTED_EDGE ( 'NONE', *, *, #1070, .F. ) ;
#4529 = VERTEX_POINT ( 'NONE', #12407 ) ;
#4530 = CARTESIAN_POINT ( 'NONE',  ( -3.468190155366909888, -1.593749999999917621, 2.319185894079683230 ) ) ;
#4531 = ORIENTED_EDGE ( 'NONE', *, *, #6717, .F. ) ;
#4532 = AXIS2_PLACEMENT_3D ( 'NONE', #11707, #9296, #5829 ) ;
#4533 = CARTESIAN_POINT ( 'NONE',  ( -4.052888063889493964, -2.499213562373234776, 0.001471977874382501914 ) ) ;
#4534 = CARTESIAN_POINT ( 'NONE',  ( 15.50000000000000000, -5.000000000000000000, -18.50000000000000000 ) ) ;
#4535 = CARTESIAN_POINT ( 'NONE',  ( 15.50000000000000000, -5.000000000000000000, 19.00000000000000000 ) ) ;
#4536 = AXIS2_PLACEMENT_3D ( 'NONE', #8812, #11076, #13401 ) ;
#4537 = CARTESIAN_POINT ( 'NONE',  ( 21.98164641901421135, -2.908542394189813650E-07, -0.3335879563140091153 ) ) ;
#4538 = FACE_OUTER_BOUND ( 'NONE', #4824, .T. ) ;
#4539 = EDGE_LOOP ( 'NONE', ( #7887, #5360 ) ) ;
#4540 = CYLINDRICAL_SURFACE ( 'NONE', #1905, 1.999999999999986233 ) ;
#4541 = VECTOR ( 'NONE', #7026, 1000.000000000000000 ) ;
#4542 = DIRECTION ( 'NONE',  ( 0.000000000000000000, -0.000000000000000000, 1.000000000000000000 ) ) ;
#4543 = VERTEX_POINT ( 'NONE', #11463 ) ;
#4544 = VECTOR ( 'NONE', #3797, 1000.000000000000000 ) ;
#4545 = LINE ( 'NONE', #13786, #9781 ) ;
#4546 = CARTESIAN_POINT ( 'NONE',  ( 2.054976948924152946, -5.156250000000162537, -3.077941148907540558 ) ) ;
#4547 = ORIENTED_EDGE ( 'NONE', *, *, #14630, .F. ) ;
#4548 = CARTESIAN_POINT ( 'NONE',  ( 2.024885806073651651, -2.741249999999974207, -3.032875982375832891 ) ) ;
#4549 = CIRCLE ( 'NONE', #12992, 1.785937500000001066 ) ;
#4550 = DIRECTION ( 'NONE',  ( 1.000000000000000000, 0.000000000000000000, 0.000000000000000000 ) ) ;
#4551 = AXIS2_PLACEMENT_3D ( 'NONE', #7900, #15167, #4559 ) ;
#4552 = DIRECTION ( 'NONE',  ( 0.000000000000000000, 0.000000000000000000, 1.000000000000000000 ) ) ;
#4553 = DIRECTION ( 'NONE',  ( 0.7071067811865425767, 0.000000000000000000, 0.7071067811865525687 ) ) ;
#4554 = CARTESIAN_POINT ( 'NONE',  ( -86.77438362643999881, 65.17411849586700612, -147.9984795835769944 ) ) ;
#4555 = FACE_OUTER_BOUND ( 'NONE', #7057, .T. ) ;
#4556 = EDGE_CURVE ( 'NONE', #7763, #8050, #3864, .T. ) ;
#4557 = LINE ( 'NONE', #11544, #11939 ) ;
#4558 = VERTEX_POINT ( 'NONE', #5585 ) ;
#4559 = DIRECTION ( 'NONE',  ( 0.000000000000000000, 0.000000000000000000, 1.000000000000000000 ) ) ;
#4560 = VECTOR ( 'NONE', #8544, 1000.000000000000114 ) ;
#4561 = ADVANCED_FACE ( 'NONE', ( #12699 ), #11237, .F. ) ;
#4562 = VECTOR ( 'NONE', #4179, 1000.000000000000114 ) ;
#4563 = ORIENTED_EDGE ( 'NONE', *, *, #9425, .T. ) ;
#4564 = VERTEX_POINT ( 'NONE', #5665 ) ;
#4565 = ORIENTED_EDGE ( 'NONE', *, *, #2693, .F. ) ;
#4566 = VERTEX_POINT ( 'NONE', #4106 ) ;
#4567 = ORIENTED_EDGE ( 'NONE', *, *, #8285, .F. ) ;
#4568 = CARTESIAN_POINT ( 'NONE',  ( 1.764499024435270735, -4.827338562373064690, 3.303210492129881715 ) ) ;
#4569 = CARTESIAN_POINT ( 'NONE',  ( 3.258191480560199693, -0.6787499999999294653, -2.178773987163739267 ) ) ;
#4570 = CARTESIAN_POINT ( 'NONE',  ( -3.970076885172157066, -2.531249999999920064, 0.7911966920917139490 ) ) ;
#4571 = AXIS2_PLACEMENT_3D ( 'NONE', #12255, #1624, #9677 ) ;
#4572 = DIRECTION ( 'NONE',  ( 0.8660254037844482555, 0.000000000000000000, 0.4999999999999831801 ) ) ;
#4573 = CARTESIAN_POINT ( 'NONE',  ( -4.353714886931050465, 2.288586792248385571, 1.459144614166439036 ) ) ;
#4574 = DIRECTION ( 'NONE',  ( 0.000000000000000000, 1.000000000000000000, 0.000000000000000000 ) ) ;
#4575 = EDGE_CURVE ( 'NONE', #13856, #5737, #392, .T. ) ;
#4576 = DIRECTION ( 'NONE',  ( 0.9961946980917453232, 0.000000000000000000, 0.08715574274766051122 ) ) ;
#4577 = ADVANCED_FACE ( 'NONE', ( #10062 ), #13646, .F. ) ;
#4578 = PLANE ( 'NONE',  #10816 ) ;
#4579 = CARTESIAN_POINT ( 'NONE',  ( -1.287538504858034338, -4.897500000000167830, -3.105113058795574421 ) ) ;
#4580 = CARTESIAN_POINT ( 'NONE',  ( -52.77438362644100067, 96.81621999649657084, -147.9984795835769944 ) ) ;
#4581 = ORIENTED_EDGE ( 'NONE', *, *, #12297, .T. ) ;
#4582 = DIRECTION ( 'NONE',  ( -0.000000000000000000, 1.000000000000000000, -0.000000000000000000 ) ) ;
#4583 = VERTEX_POINT ( 'NONE', #1216 ) ;
#4584 = ORIENTED_EDGE ( 'NONE', *, *, #1144, .T. ) ;
#4585 = VERTEX_POINT ( 'NONE', #5975 ) ;
#4586 = MECHANICAL_DESIGN_GEOMETRIC_PRESENTATION_REPRESENTATION (  '', ( #10058 ), #6586 ) ;
#4587 = CARTESIAN_POINT ( 'NONE',  ( -12.81835358098578759, -12.00000029085424025, -8.183940086454239093 ) ) ;
#4588 = VECTOR ( 'NONE', #7556, 1000.000000000000000 ) ;
#4589 = CARTESIAN_POINT ( 'NONE',  ( 2.991299100910195019, -4.663125000000096776, -1.600316903339956243 ) ) ;
#4590 = ADVANCED_FACE ( 'NONE', ( #8129 ), #13104, .F. ) ;
#4591 = DIRECTION ( 'NONE',  ( -1.000000000000000000, 0.000000000000000000, 0.000000000000000000 ) ) ;
#4592 = CARTESIAN_POINT ( 'NONE',  ( 3.031088913245534755, 0.04639863247564005727, 3.749999999999998668 ) ) ;
#4593 = FACE_OUTER_BOUND ( 'NONE', #6974, .T. ) ;
#4594 = FACE_OUTER_BOUND ( 'NONE', #13523, .T. ) ;
#4595 = DIRECTION ( 'NONE',  ( -1.000000000000000000, 0.000000000000000000, 0.000000000000000000 ) ) ;
#4596 = DIRECTION ( 'NONE',  ( -0.8660254037844387076, -0.4999999999999998890, 0.000000000000000000 ) ) ;
#4597 =( GEOMETRIC_REPRESENTATION_CONTEXT ( 3 ) GLOBAL_UNCERTAINTY_ASSIGNED_CONTEXT ( ( #15048 ) ) GLOBAL_UNIT_ASSIGNED_CONTEXT ( ( #3222, #10425, #3301 ) ) REPRESENTATION_CONTEXT ( 'NONE', 'WORKASPACE' ) );
#4598 = CARTESIAN_POINT ( 'NONE',  ( -79.02077156573416516, 103.6741184958669777, -152.4984795835769944 ) ) ;
#4599 = EDGE_CURVE ( 'NONE', #3694, #7940, #11053, .T. ) ;
#4600 = CARTESIAN_POINT ( 'NONE',  ( 35.35543536254876074, -19.31989681812820692, 6.000000000000001776 ) ) ;
#4601 =( BOUNDED_CURVE ( )  B_SPLINE_CURVE ( 3, ( #12625, #13644, #5501, #14937 ),
 .UNSPECIFIED., .F., .T. ) 
 B_SPLINE_CURVE_WITH_KNOTS ( ( 4, 4 ),
 ( 1.753449257568233444, 2.075457819525424075 ),
 .UNSPECIFIED. ) 
 CURVE ( )  GEOMETRIC_REPRESENTATION_ITEM ( )  RATIONAL_B_SPLINE_CURVE ( ( 1.000000000000000000, 0.9913778568727538154, 0.9913778568727538154, 1.000000000000000000 ) ) 
 REPRESENTATION_ITEM ( '' )  );
#4602 = MECHANICAL_DESIGN_GEOMETRIC_PRESENTATION_REPRESENTATION (  '', ( #126 ), #2357 ) ;
#4603 = VERTEX_POINT ( 'NONE', #3392 ) ;
#4604 = CARTESIAN_POINT ( 'NONE',  ( -86.77438362644001302, 99.17411849586700612, -145.4984795835769660 ) ) ;
#4605 = EDGE_CURVE ( 'NONE', #4417, #15299, #8314, .T. ) ;
#4606 = ORIENTED_EDGE ( 'NONE', *, *, #1821, .F. ) ;
#4607 = EDGE_CURVE ( 'NONE', #10402, #3944, #4716, .T. ) ;
#4608 = VERTEX_POINT ( 'NONE', #4792 ) ;
#4609 = EDGE_LOOP ( 'NONE', ( #8625, #6214, #3742, #7340 ) ) ;
#4610 = CARTESIAN_POINT ( 'NONE',  ( -1.590481721991226172, -1.687500000000021760, 3.843696589995393875 ) ) ;
#4611 = EDGE_LOOP ( 'NONE', ( #2368, #9308 ) ) ;
#4612 = AXIS2_PLACEMENT_3D ( 'NONE', #7195, #11914, #2518 ) ;
#4613 = CARTESIAN_POINT ( 'NONE',  ( 3.820744039781721391, -2.952338562373035380, 1.160108555621480519 ) ) ;
#4614 = CIRCLE ( 'NONE', #3874, 1.449999999999996403 ) ;
#4615 = EDGE_CURVE ( 'NONE', #13053, #4566, #48, .T. ) ;
#4616 = CIRCLE ( 'NONE', #14993, 2.093999815491831562 ) ;
#4617 = PLANE ( 'NONE',  #11936 ) ;
#4618 = CARTESIAN_POINT ( 'NONE',  ( -69.77438362644001302, 82.17411849586700612, -83.44847958357698303 ) ) ;
#4619 = DIRECTION ( 'NONE',  ( 0.000000000000000000, 1.000000000000000000, 0.000000000000000000 ) ) ;
#4620 = EDGE_CURVE ( 'NONE', #6732, #1190, #10516, .T. ) ;
#4621 = PRODUCT_DEFINITION_SHAPE ( 'NONE', 'NONE',  #15337 ) ;
#4622 = DIRECTION ( 'NONE',  ( 0.000000000000000000, -1.000000000000000000, 0.000000000000000000 ) ) ;
#4623 = ORIENTED_EDGE ( 'NONE', *, *, #4016, .T. ) ;
#4624 = AXIS2_PLACEMENT_3D ( 'NONE', #11403, #5528, #10229 ) ;
#4625 = CARTESIAN_POINT ( 'NONE',  ( 3.557408335254829801, -5.205290677742872241, -0.3931923741407351014 ) ) ;
#4626 = CARTESIAN_POINT ( 'NONE',  ( 10.10406781373725948, 10.99999970914572778, 69.08979243323354069 ) ) ;
#4627 = VECTOR ( 'NONE', #7864, 1000.000000000000000 ) ;
#4628 = CIRCLE ( 'NONE', #10780, 1.999999999999986233 ) ;
#4629 = DIRECTION ( 'NONE',  ( 1.000000000000000000, 0.000000000000000000, 0.000000000000000000 ) ) ;
#4630 = VERTEX_POINT ( 'NONE', #13020 ) ;
#4631 =( LENGTH_UNIT ( ) NAMED_UNIT ( * ) SI_UNIT ( .MILLI., .METRE. ) );
#4632 = CARTESIAN_POINT ( 'NONE',  ( -3.916933349122203367, -0.1162499999999876271, 0.7806084585172713419 ) ) ;
#4633 = VERTEX_POINT ( 'NONE', #4642 ) ;
#4634 = AXIS2_PLACEMENT_3D ( 'NONE', #12072, #14458, #12215 ) ;
#4635 = CARTESIAN_POINT ( 'NONE',  ( 0.3573659033054957801, -2.819374999999921805, -3.618812876704415427 ) ) ;
#4636 = DIRECTION ( 'NONE',  ( 0.000000000000000000, 0.000000000000000000, -1.000000000000000000 ) ) ;
#4637 = CIRCLE ( 'NONE', #7375, 0.8000000000000052625 ) ;
#4638 = DIRECTION ( 'NONE',  ( 1.000000000000000000, 0.000000000000000000, 0.000000000000000000 ) ) ;
#4639 = DIRECTION ( 'NONE',  ( 0.000000000000000000, 1.000000000000000000, 0.000000000000000000 ) ) ;
#4640 = DIRECTION ( 'NONE',  ( 0.000000000000000000, 1.000000000000000000, 0.000000000000000000 ) ) ;
#4641 = FACE_OUTER_BOUND ( 'NONE', #15134, .T. ) ;
#4642 = CARTESIAN_POINT ( 'NONE',  ( -2.514916625122314731, 4.927357795815630048, 0.000000000000000000 ) ) ;
#4643 = CYLINDRICAL_SURFACE ( 'NONE', #7244, 5.499999999999998224 ) ;
#4644 = ORIENTED_EDGE ( 'NONE', *, *, #4708, .T. ) ;
#4645 = DIRECTION ( 'NONE',  ( 0.000000000000000000, 0.000000000000000000, -1.000000000000000000 ) ) ;
#4646 = CIRCLE ( 'NONE', #13079, 16.00000000000000000 ) ;
#4647 = ORIENTED_EDGE ( 'NONE', *, *, #12754, .F. ) ;
#4648 = AXIS2_PLACEMENT_3D ( 'NONE', #1468, #9751, #5037 ) ;
#4649 = EDGE_LOOP ( 'NONE', ( #11202, #14563, #13968, #10074 ) ) ;
#4650 = CARTESIAN_POINT ( 'NONE',  ( -3.468991550463838891, -4.085000000000062137, -0.0008868951686453910126 ) ) ;
#4651 = ORIENTED_EDGE ( 'NONE', *, *, #10171, .T. ) ;
#4652 = ORIENTED_EDGE ( 'NONE', *, *, #9056, .T. ) ;
#4653 = ORIENTED_EDGE ( 'NONE', *, *, #7651, .T. ) ;
#4654 = CARTESIAN_POINT ( 'NONE',  ( -2.916346042413609840, -4.608588562373151731, 2.395174355888781026 ) ) ;
#4655 = CARTESIAN_POINT ( 'NONE',  ( -69.77438362644001302, 82.17411849586700612, -80.14847958357698587 ) ) ;
#4656 = FACE_OUTER_BOUND ( 'NONE', #2731, .T. ) ;
#4657 = CARTESIAN_POINT ( 'NONE',  ( 66.41329019055577021, 5.000000000000000000, 89.50956111919107627 ) ) ;
#4658 = EDGE_CURVE ( 'NONE', #13129, #5656, #5601, .T. ) ;
#4659 = CYLINDRICAL_SURFACE ( 'NONE', #7118, 2.750000000000002665 ) ;
#4660 = AXIS2_PLACEMENT_3D ( 'NONE', #8924, #9927, #1867 ) ;
#4661 = DIRECTION ( 'NONE',  ( -1.284980352575412699E-16, -0.000000000000000000, -1.000000000000000000 ) ) ;
#4662 = CARTESIAN_POINT ( 'NONE',  ( -50.27438362643999881, 65.17411849586700612, -145.2984795835770058 ) ) ;
#4663 = CYLINDRICAL_SURFACE ( 'NONE', #11798, 5.500000000000005329 ) ;
#4664 = CARTESIAN_POINT ( 'NONE',  ( 3.384491019838401726, -4.600625000000129639, -0.3324735777645301260 ) ) ;
#4665 = CARTESIAN_POINT ( 'NONE',  ( -4.486254801108946033, -12.00000029085428110, 69.62284035768028900 ) ) ;
#4666 = VERTEX_POINT ( 'NONE', #6964 ) ;
#4667 = DIRECTION ( 'NONE',  ( -9.422394424380278809E-16, 1.000000000000000000, -0.000000000000000000 ) ) ;
#4668 = VERTEX_POINT ( 'NONE', #2222 ) ;
#4669 = EDGE_LOOP ( 'NONE', ( #14315, #1608, #6832 ) ) ;
#4670 = ORIENTED_EDGE ( 'NONE', *, *, #11417, .F. ) ;
#4671 = CONICAL_SURFACE ( 'NONE', #2933, 3.250000000000015987, 0.4363323129985828275 ) ;
#4672 = DIRECTION ( 'NONE',  ( -1.000000000000000000, 0.000000000000000000, 0.000000000000000000 ) ) ;
#4673 = PRODUCT_RELATED_PRODUCT_CATEGORY ( 'part', '', ( #12915 ) ) ;
#4674 = ADVANCED_FACE ( 'NONE', ( #4555 ), #4853, .T. ) ;
#4675 = CARTESIAN_POINT ( 'NONE',  ( -0.6956252696767697419, -3.303750000000123421, 3.503916970779588969 ) ) ;
#4676 = PLANE ( 'NONE',  #12795 ) ;
#4677 = DIRECTION ( 'NONE',  ( -1.000000000000000000, 0.000000000000000000, 0.000000000000000000 ) ) ;
#4678 = LINE ( 'NONE', #12739, #8483 ) ;
#4679 = EDGE_CURVE ( 'NONE', #13729, #10133, #1377, .T. ) ;
#4680 = DIRECTION ( 'NONE',  ( 0.000000000000000000, 1.000000000000000000, 0.000000000000000000 ) ) ;
#4681 = FACE_OUTER_BOUND ( 'NONE', #11552, .T. ) ;
#4682 = CARTESIAN_POINT ( 'NONE',  ( -7.760341206926691271, 5.861171052203402648E-16, 49.67725299158860253 ) ) ;
#4683 = CARTESIAN_POINT ( 'NONE',  ( -86.77438362643999881, 67.53201699523744139, -147.9984795835769944 ) ) ;
#4684 = CARTESIAN_POINT ( 'NONE',  ( -46.58670980944423690, 5.000000000000000000, 91.50956111919106206 ) ) ;
#4685 = AXIS2_PLACEMENT_3D ( 'NONE', #12168, #9909, #8674 ) ;
#4686 = ORIENTED_EDGE ( 'NONE', *, *, #12644, .T. ) ;
#4687 = DIRECTION ( 'NONE',  ( 1.000000000000000000, 0.000000000000000000, 0.000000000000000000 ) ) ;
#4688 = VERTEX_POINT ( 'NONE', #7049 ) ;
#4689 = EDGE_LOOP ( 'NONE', ( #9003, #10685, #7081, #2947 ) ) ;
#4690 = CARTESIAN_POINT ( 'NONE',  ( 0.8505843571400346637, -0.2187500000000167921, -4.270207479395898176 ) ) ;
#4691 = VERTEX_POINT ( 'NONE', #11769 ) ;
#4692 = ADVANCED_FACE ( 'NONE', ( #15089 ), #2128, .T. ) ;
#4693 = CARTESIAN_POINT ( 'NONE',  ( 0.3927583221442342287, -2.764838562373139741, 3.998546384597275516 ) ) ;
#4694 = AXIS2_PLACEMENT_3D ( 'NONE', #8890, #3152, #735 ) ;
#4695 = CARTESIAN_POINT ( 'NONE',  ( -84.73238362643999722, 65.17411849586700612, -147.9984795835769944 ) ) ;
#4696 = ADVANCED_FACE ( 'NONE', ( #14165, #2379 ), #11926, .T. ) ;
#4697 = LINE ( 'NONE', #3682, #5111 ) ;
#4698 = CARTESIAN_POINT ( 'NONE',  ( 4.130341191321588390, 2.356280171323994921, -1.846039204036428849 ) ) ;
#4699 = FACE_OUTER_BOUND ( 'NONE', #14555, .T. ) ;
#4700 = ORIENTED_EDGE ( 'NONE', *, *, #7275, .F. ) ;
#4701 = FACE_OUTER_BOUND ( 'NONE', #4242, .T. ) ;
#4702 = DIRECTION ( 'NONE',  ( -1.000000000000000000, 0.000000000000000000, 0.000000000000000000 ) ) ;
#4703 = ADVANCED_FACE ( 'NONE', ( #7205 ), #9551, .T. ) ;
#4704 = EDGE_LOOP ( 'NONE', ( #6404, #6548, #12515, #4245 ) ) ;
#4705 = SURFACE_STYLE_USAGE ( .BOTH. , #6122 ) ;
#4706 = CARTESIAN_POINT ( 'NONE',  ( 3.837491448225466062, -3.984374999999830802, 0.3765428855677108166 ) ) ;
#4707 = EDGE_LOOP ( 'NONE', ( #11180, #4209, #5558, #13731, #1441 ) ) ;
#4708 = EDGE_CURVE ( 'NONE', #13728, #13838, #4475, .T. ) ;
#4709 = CARTESIAN_POINT ( 'NONE',  ( -2.355664480073890399, -2.225624999999979092, 2.872538697791624518 ) ) ;
#4710 = EDGE_CURVE ( 'NONE', #7835, #2560, #3777, .T. ) ;
#4711 = EDGE_CURVE ( 'NONE', #13765, #1574, #1139, .T. ) ;
#4712 = CARTESIAN_POINT ( 'NONE',  ( -86.77438362644100778, 99.17411849586700612, -145.2984795835770058 ) ) ;
#4713 = DIRECTION ( 'NONE',  ( -1.747085166004344019E-15, 1.000000000000000000, -0.000000000000000000 ) ) ;
#4714 = DIRECTION ( 'NONE',  ( -2.551930889570659960E-15, 1.000000000000000000, 0.000000000000000000 ) ) ;
#4715 = PRESENTATION_STYLE_ASSIGNMENT (( #9278 ) ) ;
#4716 = LINE ( 'NONE', #12863, #8059 ) ;
#4717 = CARTESIAN_POINT ( 'NONE',  ( -12.81835358098578403, 12.49999970914576153, -8.775548064764198131 ) ) ;
#4718 = ORIENTED_EDGE ( 'NONE', *, *, #11521, .F. ) ;
#4719 = DIRECTION ( 'NONE',  ( 0.000000000000000000, 0.000000000000000000, -1.000000000000000000 ) ) ;
#4720 = VERTEX_POINT ( 'NONE', #1684 ) ;
#4721 = FACE_OUTER_BOUND ( 'NONE', #1970, .T. ) ;
#4722 = CARTESIAN_POINT ( 'NONE',  ( 2.642398951855386979, -4.475625000000026610, 2.166914421091104881 ) ) ;
#4723 = ORIENTED_EDGE ( 'NONE', *, *, #6528, .F. ) ;
#4724 = ORIENTED_EDGE ( 'NONE', *, *, #13810, .F. ) ;
#4725 = ORIENTED_EDGE ( 'NONE', *, *, #11048, .T. ) ;
#4726 = CARTESIAN_POINT ( 'NONE',  ( 3.694831845485670119, -3.952338562372989195, 1.119339768987546169 ) ) ;
#4727 = CARTESIAN_POINT ( 'NONE',  ( 22.58164641901421632, 12.59999970914575940, -8.183940086454237317 ) ) ;
#4728 = DIRECTION ( 'NONE',  ( 0.8660254037844387076, 2.210036979070412685E-15, 0.4999999999999999445 ) ) ;
#4729 = LINE ( 'NONE', #11634, #11217 ) ;
#4730 = DIRECTION ( 'NONE',  ( 0.000000000000000000, 1.000000000000000000, 0.000000000000000000 ) ) ;
#4731 = DIRECTION ( 'NONE',  ( -1.000000000000000000, 0.000000000000000000, 0.000000000000000000 ) ) ;
#4732 = DIRECTION ( 'NONE',  ( 1.000000000000000000, 0.000000000000000000, 0.000000000000000000 ) ) ;
#4733 = DIRECTION ( 'NONE',  ( 0.000000000000000000, 0.000000000000000000, 1.000000000000000000 ) ) ;
#4734 = CARTESIAN_POINT ( 'NONE',  ( 1.656526992905777318, -3.756875000000012399, -3.097233728230734062 ) ) ;
#4735 = DIRECTION ( 'NONE',  ( -1.000000000000000000, 0.000000000000000000, -0.000000000000000000 ) ) ;
#4736 = ORIENTED_EDGE ( 'NONE', *, *, #10578, .T. ) ;
#4737 = CARTESIAN_POINT ( 'NONE',  ( 10.10406781373725771, -85.69524470659703752, 69.08979243323349806 ) ) ;
#4738 = EDGE_LOOP ( 'NONE', ( #2916, #13198 ) ) ;
#4739 = AXIS2_PLACEMENT_3D ( 'NONE', #14692, #14916, #2836 ) ;
#4740 = ORIENTED_EDGE ( 'NONE', *, *, #6592, .T. ) ;
#4741 = ORIENTED_EDGE ( 'NONE', *, *, #9718, .F. ) ;
#4742 = AXIS2_PLACEMENT_3D ( 'NONE', #11681, #6959, #10512 ) ;
#4743 = CARTESIAN_POINT ( 'NONE',  ( -69.77438362644001302, 82.17411849586700612, -93.49847958357699440 ) ) ;
#4744 = CARTESIAN_POINT ( 'NONE',  ( -63.90163006221920483, 66.22072495173567575, -81.84847958357697451 ) ) ;
#4745 = DIRECTION ( 'NONE',  ( 0.000000000000000000, 1.000000000000000000, 0.000000000000000000 ) ) ;
#4746 = FACE_OUTER_BOUND ( 'NONE', #6342, .T. ) ;
#4747 = DIRECTION ( 'NONE',  ( -1.000000000000000000, 0.000000000000000000, 0.000000000000000000 ) ) ;
#4748 = VECTOR ( 'NONE', #1661, 1000.000000000000000 ) ;
#4749 = DIRECTION ( 'NONE',  ( 0.7071067811865505703, -0.7071067811865444641, -8.659560562354948882E-17 ) ) ;
#4750 = LINE ( 'NONE', #1102, #833 ) ;
#4751 = DIRECTION ( 'NONE',  ( 0.000000000000000000, 0.000000000000000000, -1.000000000000000000 ) ) ;
#4752 = CARTESIAN_POINT ( 'NONE',  ( -2.598076211353319565, 1.678847577293365978, -4.499999999999999112 ) ) ;
#4753 = LINE ( 'NONE', #4684, #11725 ) ;
#4754 = AXIS2_PLACEMENT_3D ( 'NONE', #1110, #14138, #15296 ) ;
#4755 = VERTEX_POINT ( 'NONE', #202 ) ;
#4756 = CARTESIAN_POINT ( 'NONE',  ( -57.27438362644000591, 99.17411849586700612, -152.4984795835769944 ) ) ;
#4757 = AXIS2_PLACEMENT_3D ( 'NONE', #13866, #12939, #8279 ) ;
#4758 = ADVANCED_FACE ( 'NONE', ( #10842 ), #5022, .F. ) ;
#4759 = VERTEX_POINT ( 'NONE', #1524 ) ;
#4760 = ORIENTED_EDGE ( 'NONE', *, *, #1668, .F. ) ;
#4761 = CARTESIAN_POINT ( 'NONE',  ( -16.75000000000000000, -0.3156864504677179273, -22.74361999681790536 ) ) ;
#4762 = EDGE_CURVE ( 'NONE', #11586, #10105, #14765, .T. ) ;
#4763 = VECTOR ( 'NONE', #6088, 1000.000000000000000 ) ;
#4764 = CARTESIAN_POINT ( 'NONE',  ( -4.425813417735612987, 0.4843740197764026534, 0.4347324592064809035 ) ) ;
#4765 = ORIENTED_EDGE ( 'NONE', *, *, #9772, .T. ) ;
#4766 = CARTESIAN_POINT ( 'NONE',  ( 1.616006145108879855, -1.186713562373049813, -3.905372697150129468 ) ) ;
#4767 = AXIS2_PLACEMENT_3D ( 'NONE', #7786, #8075, #13969 ) ;
#4768 = LINE ( 'NONE', #9562, #2270 ) ;
#4769 = CARTESIAN_POINT ( 'NONE',  ( -69.77438362644001302, 84.67411849586700612, -51.99847958357699440 ) ) ;
#4770 = CARTESIAN_POINT ( 'NONE',  ( -52.77438362644100067, 96.81621999649657084, -150.4984795835770228 ) ) ;
#4771 = DIRECTION ( 'NONE',  ( 0.000000000000000000, 0.000000000000000000, -1.000000000000000000 ) ) ;
#4772 = ORIENTED_EDGE ( 'NONE', *, *, #5193, .T. ) ;
#4773 = DIRECTION ( 'NONE',  ( -0.08715574274766176022, -4.320305823558445788E-16, 0.9961946980917453232 ) ) ;
#4774 = EDGE_CURVE ( 'NONE', #6230, #4906, #15246, .T. ) ;
#4775 = CARTESIAN_POINT ( 'NONE',  ( 16.12213235758455809, 11.99999970914575798, 0.3029999356681916667 ) ) ;
#4776 = VECTOR ( 'NONE', #2686, 1000.000000000000000 ) ;
#4777 = ORIENTED_EDGE ( 'NONE', *, *, #15300, .F. ) ;
#4778 = EDGE_CURVE ( 'NONE', #6631, #8647, #10991, .T. ) ;
#4779 = CARTESIAN_POINT ( 'NONE',  ( 0.3668491701747067513, -4.765624999999817923, 3.734637934618871391 ) ) ;
#4780 = EDGE_LOOP ( 'NONE', ( #15062, #5617, #11700, #4528 ) ) ;
#4781 = TOROIDAL_SURFACE ( 'NONE', #6774, 2.700000000000000178, 0.2000000000000000111 ) ;
#4782 = CARTESIAN_POINT ( 'NONE',  ( -3.865847815970003154, -1.085000000000063469, -0.001011349278461548453 ) ) ;
#4783 = DIRECTION ( 'NONE',  ( 0.000000000000000000, 0.000000000000000000, -1.000000000000000000 ) ) ;
#4784 = CARTESIAN_POINT ( 'NONE',  ( -1.578751687972824502, -5.349924609423814204, 2.979769298184874682 ) ) ;
#4785 = EDGE_CURVE ( 'NONE', #9369, #5220, #8341, .T. ) ;
#4786 = ADVANCED_FACE ( 'NONE', ( #4947 ), #7283, .T. ) ;
#4787 = DIRECTION ( 'NONE',  ( -1.224646799147353947E-16, 1.000000000000000000, 0.000000000000000000 ) ) ;
#4788 = DIRECTION ( 'NONE',  ( -1.747085166004344019E-15, 1.000000000000000000, -0.000000000000000000 ) ) ;
#4789 = AXIS2_PLACEMENT_3D ( 'NONE', #15194, #4582, #9307 ) ;
#4790 = CARTESIAN_POINT ( 'NONE',  ( -54.81638362644100226, 100.3530677455522238, -147.9984795835769944 ) ) ;
#4791 = CARTESIAN_POINT ( 'NONE',  ( 2.517719788909356549, -5.362458399163725353, 2.218656285138580486 ) ) ;
#4792 = CARTESIAN_POINT ( 'NONE',  ( -15.50000000000000000, -5.000000000000000000, -26.50000000000000000 ) ) ;
#4793 = EDGE_CURVE ( 'NONE', #2784, #14784, #2631, .T. ) ;
#4794 = VECTOR ( 'NONE', #7853, 1000.000000000000000 ) ;
#4795 = ORIENTED_EDGE ( 'NONE', *, *, #13781, .T. ) ;
#4796 = CARTESIAN_POINT ( 'NONE',  ( -52.77438362643999881, 65.17411849586700612, -150.4984795835770228 ) ) ;
#4797 = ORIENTED_EDGE ( 'NONE', *, *, #14443, .T. ) ;
#4798 = EDGE_CURVE ( 'NONE', #6810, #1528, #4004, .T. ) ;
#4799 = DIRECTION ( 'NONE',  ( 0.000000000000000000, 0.000000000000000000, -1.000000000000000000 ) ) ;
#4800 = EDGE_CURVE ( 'NONE', #2099, #9156, #8589, .T. ) ;
#4801 = CARTESIAN_POINT ( 'NONE',  ( -1.054465238365617452, -2.881875000000049702, -3.471494129216006197 ) ) ;
#4802 = ORIENTED_EDGE ( 'NONE', *, *, #9354, .F. ) ;
#4803 = EDGE_LOOP ( 'NONE', ( #6043, #4092, #2080 ) ) ;
#4804 = AXIS2_PLACEMENT_3D ( 'NONE', #1250, #10481, #13979 ) ;
#4805 = AXIS2_PLACEMENT_3D ( 'NONE', #3395, #4337, #9059 ) ;
#4806 = ORIENTED_EDGE ( 'NONE', *, *, #876, .F. ) ;
#4807 = DIRECTION ( 'NONE',  ( 0.000000000000000000, 0.000000000000000000, -1.000000000000000000 ) ) ;
#4808 = CIRCLE ( 'NONE', #6066, 3.968749999999992895 ) ;
#4809 = EDGE_CURVE ( 'NONE', #6326, #6998, #6371, .T. ) ;
#4810 = CARTESIAN_POINT ( 'NONE',  ( -69.77438362644001302, 99.17411849586700612, -81.84847958357698872 ) ) ;
#4811 = CARTESIAN_POINT ( 'NONE',  ( -59.27438362644000591, 82.17411849586700612, -80.44847958357698303 ) ) ;
#4812 = LINE ( 'NONE', #14186, #4173 ) ;
#4813 = SURFACE_STYLE_USAGE ( .BOTH. , #7532 ) ;
#4814 = DIRECTION ( 'NONE',  ( -1.000000000000000000, -0.000000000000000000, -0.000000000000000000 ) ) ;
#4815 = AXIS2_PLACEMENT_3D ( 'NONE', #7717, #1804, #11422 ) ;
#4816 = VECTOR ( 'NONE', #4963, 1000.000000000000000 ) ;
#4817 = ADVANCED_FACE ( 'NONE', ( #6206 ), #9584, .F. ) ;
#4818 = CARTESIAN_POINT ( 'NONE',  ( -0.6836773592642079178, -3.866249999999994635, -3.430425219284937821 ) ) ;
#4819 = CARTESIAN_POINT ( 'NONE',  ( -57.27438362644000591, 99.17411849586700612, -86.49847958357699440 ) ) ;
#4820 = EDGE_LOOP ( 'NONE', ( #7994, #516 ) ) ;
#4821 = DIRECTION ( 'NONE',  ( 0.000000000000000000, 0.000000000000000000, -1.000000000000000000 ) ) ;
#4822 = VERTEX_POINT ( 'NONE', #1606 ) ;
#4823 = EDGE_LOOP ( 'NONE', ( #5910, #12037 ) ) ;
#4824 = EDGE_LOOP ( 'NONE', ( #3255, #1509, #14171, #6632 ) ) ;
#4825 = CARTESIAN_POINT ( 'NONE',  ( -0.6310725616347281353, 2.041549731959705837E-17, 25.55790572381511794 ) ) ;
#4826 = CIRCLE ( 'NONE', #9022, 16.50000000000000000 ) ;
#4827 = AXIS2_PLACEMENT_3D ( 'NONE', #8766, #303, #6533 ) ;
#4828 = CARTESIAN_POINT ( 'NONE',  ( -0.7073002561900942897, -2.866249999999988418, -3.560643744722076232 ) ) ;
#4829 = AXIS2_PLACEMENT_3D ( 'NONE', #8730, #15129, #9018 ) ;
#4830 = CARTESIAN_POINT ( 'NONE',  ( -88.81638362644100937, 97.99516924618178848, -147.9984795835769944 ) ) ;
#4831 = CARTESIAN_POINT ( 'NONE',  ( 2.598076211353309350, 2.375000000000006661, 4.500000000000000000 ) ) ;
#4832 = CARTESIAN_POINT ( 'NONE',  ( -16.75000000000000000, -2.500000000000000000, -21.77831216351300014 ) ) ;
#4833 = DIRECTION ( 'NONE',  ( 0.000000000000000000, 1.000000000000000000, 0.000000000000000000 ) ) ;
#4834 = FACE_OUTER_BOUND ( 'NONE', #14723, .T. ) ;
#4835 = CARTESIAN_POINT ( 'NONE',  ( 0.000000000000000000, 0.000000000000000000, -79.49847958357700861 ) ) ;
#4836 = DIRECTION ( 'NONE',  ( 0.000000000000000000, 0.000000000000000000, 1.000000000000000000 ) ) ;
#4837 = DIRECTION ( 'NONE',  ( -0.000000000000000000, 1.000000000000000000, -0.000000000000000000 ) ) ;
#4838 = DIRECTION ( 'NONE',  ( 0.4999999999999998890, -0.8660254037844387076, 0.000000000000000000 ) ) ;
#4839 = ORIENTED_EDGE ( 'NONE', *, *, #6098, .T. ) ;
#4840 = LINE ( 'NONE', #409, #12814 ) ;
#4841 = VERTEX_POINT ( 'NONE', #14322 ) ;
#4842 = ORIENTED_EDGE ( 'NONE', *, *, #12745, .F. ) ;
#4843 = ORIENTED_EDGE ( 'NONE', *, *, #14162, .T. ) ;
#4844 = CIRCLE ( 'NONE', #13270, 0.5999999999999999778 ) ;
#4845 = DIRECTION ( 'NONE',  ( 0.000000000000000000, 1.000000000000000000, 0.000000000000000000 ) ) ;
#4846 = CARTESIAN_POINT ( 'NONE',  ( 2.793566534610028018, 0.1406250000000374423, 3.401478000866359430 ) ) ;
#4847 = EDGE_LOOP ( 'NONE', ( #1223, #2115 ) ) ;
#4848 = CARTESIAN_POINT ( 'NONE',  ( -1.205651417374353773, -1.702338562373074904, 3.979684766797042528 ) ) ;
#4849 = CIRCLE ( 'NONE', #8311, 4.000000000000000888 ) ;
#4850 = PLANE ( 'NONE',  #5499 ) ;
#4851 = DIRECTION ( 'NONE',  ( 0.000000000000000000, 0.000000000000000000, -1.000000000000000000 ) ) ;
#4852 = DIRECTION ( 'NONE',  ( 0.000000000000000000, 1.000000000000000000, 0.000000000000000000 ) ) ;
#4853 = TOROIDAL_SURFACE ( 'NONE', #6837, 1.200000000000000178, 0.6000000000000000888 ) ;
#4854 = EDGE_CURVE ( 'NONE', #10808, #10427, #10912, .T. ) ;
#4855 = CARTESIAN_POINT ( 'NONE',  ( -35.58670980944424400, 5.000000000000001776, 129.5095611191910621 ) ) ;
#4856 = EDGE_LOOP ( 'NONE', ( #2281, #2645, #4524, #6163 ) ) ;
#4857 = LINE ( 'NONE', #2676, #5892 ) ;
#4858 = LINE ( 'NONE', #9493, #9211 ) ;
#4859 = VECTOR ( 'NONE', #11203, 1000.000000000000114 ) ;
#4860 = SHAPE_DEFINITION_REPRESENTATION ( #7702, #14417 ) ;
#4861 = ORIENTED_EDGE ( 'NONE', *, *, #6785, .F. ) ;
#4862 = AXIS2_PLACEMENT_3D ( 'NONE', #12840, #1903, #3215 ) ;
#4863 =( LENGTH_UNIT ( ) NAMED_UNIT ( * ) SI_UNIT ( .MILLI., .METRE. ) );
#4864 = CARTESIAN_POINT ( 'NONE',  ( -2.475833455637627800, -3.640624999999937383, 3.015200003105952042 ) ) ;
#4865 = ORIENTED_EDGE ( 'NONE', *, *, #15269, .T. ) ;
#4866 = AXIS2_PLACEMENT_3D ( 'NONE', #12392, #1750, #584 ) ;
#4867 = APPLICATION_CONTEXT ( 'automotive_design' ) ;
#4868 = CARTESIAN_POINT ( 'NONE',  ( 3.402892030661166523, -0.5020034630054815983, 1.955069923487531947 ) ) ;
#4869 = ADVANCED_FACE ( 'NONE', ( #12007 ), #5107, .F. ) ;
#4870 = CARTESIAN_POINT ( 'NONE',  ( -2.636171414473165608, -5.322656474840649743, 2.174809469211999691 ) ) ;
#4871 = CIRCLE ( 'NONE', #1149, 2.093999815491831562 ) ;
#4872 = LINE ( 'NONE', #1368, #5577 ) ;
#4873 = ADVANCED_FACE ( 'NONE', ( #6359 ), #9822, .T. ) ;
#4874 = CIRCLE ( 'NONE', #10560, 10.49999999999999467 ) ;
#4875 = FACE_OUTER_BOUND ( 'NONE', #11772, .T. ) ;
#4876 = PLANE ( 'NONE',  #2796 ) ;
#4877 = AXIS2_PLACEMENT_3D ( 'NONE', #6777, #3268, #11274 ) ;
#4878 = DIRECTION ( 'NONE',  ( 0.000000000000000000, 0.000000000000000000, -1.000000000000000000 ) ) ;
#4879 = EDGE_LOOP ( 'NONE', ( #113, #72 ) ) ;
#4880 = CARTESIAN_POINT ( 'NONE',  ( -75.01311196519617397, 67.29799558322736175, -83.44847958357698303 ) ) ;
#4881 = DIRECTION ( 'NONE',  ( 0.000000000000000000, 0.000000000000000000, 1.000000000000000000 ) ) ;
#4882 = ORIENTED_EDGE ( 'NONE', *, *, #10381, .F. ) ;
#4883 = PRODUCT_DEFINITION_SHAPE ( 'NONE', 'NONE',  #3235 ) ;
#4884 = DIRECTION ( 'NONE',  ( 0.000000000000000000, 0.000000000000000000, 1.000000000000000000 ) ) ;
#4885 = CARTESIAN_POINT ( 'NONE',  ( 3.667419683216787352, -2.585000000000003517, 0.0009491222189902254192 ) ) ;
#4886 = ORIENTED_EDGE ( 'NONE', *, *, #11424, .F. ) ;
#4887 = VECTOR ( 'NONE', #12767, 1000.000000000000000 ) ;
#4888 = VERTEX_POINT ( 'NONE', #13563 ) ;
#4889 = EDGE_LOOP ( 'NONE', ( #2195, #14770 ) ) ;
#4890 = AXIS2_PLACEMENT_3D ( 'NONE', #619, #14738, #10225 ) ;
#4891 = DIRECTION ( 'NONE',  ( 0.000000000000000000, 0.000000000000000000, -1.000000000000000000 ) ) ;
#4892 = EDGE_CURVE ( 'NONE', #9382, #1688, #4616, .T. ) ;
#4893 = CARTESIAN_POINT ( 'NONE',  ( 22.58164641901421632, -12.00000029085424202, -0.3335879563140091153 ) ) ;
#4894 = ADVANCED_FACE ( 'NONE', ( #9968 ), #512, .T. ) ;
#4895 = EDGE_CURVE ( 'NONE', #6527, #7325, #4168, .T. ) ;
#4896 = DIRECTION ( 'NONE',  ( 0.000000000000000000, 0.000000000000000000, -1.000000000000000000 ) ) ;
#4897 = DIRECTION ( 'NONE',  ( 0.000000000000000000, 1.734723475976805517E-15, -1.000000000000000000 ) ) ;
#4898 = VECTOR ( 'NONE', #4155, 1000.000000000000114 ) ;
#4899 = DIRECTION ( 'NONE',  ( -1.000000000000000000, -0.000000000000000000, -0.000000000000000000 ) ) ;
#4900 = CARTESIAN_POINT ( 'NONE',  ( -3.527726845254099075, -3.116249999999919140, 0.7030635791094290710 ) ) ;
#4901 = CARTESIAN_POINT ( 'NONE',  ( -15.50000000000000000, -1.037157890325000054, 22.50000000000000000 ) ) ;
#4902 = ORIENTED_EDGE ( 'NONE', *, *, #2519, .T. ) ;
#4903 = CARTESIAN_POINT ( 'NONE',  ( -52.77438362644100067, 99.17411849586700612, -147.9984795835769944 ) ) ;
#4904 = ORIENTED_EDGE ( 'NONE', *, *, #14622, .T. ) ;
#4905 = EDGE_CURVE ( 'NONE', #14839, #3822, #8892, .T. ) ;
#4906 = VERTEX_POINT ( 'NONE', #10045 ) ;
#4907 = EDGE_LOOP ( 'NONE', ( #7804, #14067, #2809, #14348 ) ) ;
#4908 = EDGE_LOOP ( 'NONE', ( #12949, #2662, #7876, #3287 ) ) ;
#4909 = EDGE_CURVE ( 'NONE', #2233, #6527, #737, .T. ) ;
#4910 = AXIS2_PLACEMENT_3D ( 'NONE', #8396, #8321, #8239 ) ;
#4911 = CARTESIAN_POINT ( 'NONE',  ( -86.77438362643999881, 62.81621999649657084, -147.9984795835769944 ) ) ;
#4912 = CARTESIAN_POINT ( 'NONE',  ( 3.430119610663647567, -5.062500000000104805, -1.422280051980938431 ) ) ;
#4913 = FACE_OUTER_BOUND ( 'NONE', #2870, .T. ) ;
#4914 = LINE ( 'NONE', #3665, #11306 ) ;
#4915 = ADVANCED_FACE ( 'NONE', ( #11215 ), #5490, .F. ) ;
#4916 = CARTESIAN_POINT ( 'NONE',  ( -50.73238362643999722, 66.35306774555222376, -147.9984795835769944 ) ) ;
#4917 = CARTESIAN_POINT ( 'NONE',  ( -56.52438362644099357, 99.17411849586700612, -150.4984795835770228 ) ) ;
#4918 = CARTESIAN_POINT ( 'NONE',  ( 14.05000000000000249, -0.2000000000000000111, 22.50000000000000000 ) ) ;
#4919 = LINE ( 'NONE', #13141, #12778 ) ;
#4920 = CARTESIAN_POINT ( 'NONE',  ( -69.43626855224066219, 89.17411849586700612, -43.99847958365484146 ) ) ;
#4921 = EDGE_LOOP ( 'NONE', ( #9133, #10212, #7141, #2286 ) ) ;
#4922 = CARTESIAN_POINT ( 'NONE',  ( 16.75446144793115977, -11.78527509924292715, 0.2672796091214772463 ) ) ;
#4923 = VERTEX_POINT ( 'NONE', #13703 ) ;
#4924 = CIRCLE ( 'NONE', #2683, 1.999999999999988010 ) ;
#4925 = VERTEX_POINT ( 'NONE', #7884 ) ;
#4926 = FACE_BOUND ( 'NONE', #3785, .T. ) ;
#4927 = CARTESIAN_POINT ( 'NONE',  ( 3.398568864256001909, 0.1093749999999974742, 2.790657398000633727 ) ) ;
#4928 = CARTESIAN_POINT ( 'NONE',  ( -1.984936106024998814, -1.327338562373031383, -3.710328542583766431 ) ) ;
#4929 = DIRECTION ( 'NONE',  ( 0.000000000000000000, 1.000000000000000000, 0.000000000000000000 ) ) ;
#4930 = CARTESIAN_POINT ( 'NONE',  ( -69.77438362644001302, 82.17411849586700612, -150.4984795835769944 ) ) ;
#4931 = CYLINDRICAL_SURFACE ( 'NONE', #14762, 1.999999999999986233 ) ;
#4932 = CARTESIAN_POINT ( 'NONE',  ( 17.18164641901421419, -12.00000029085424025, 0.8664120436859875651 ) ) ;
#4933 = CARTESIAN_POINT ( 'NONE',  ( -69.77438362644001302, 99.17411849586700612, -81.84847958357698872 ) ) ;
#4934 = ORIENTED_EDGE ( 'NONE', *, *, #8768, .T. ) ;
#4935 = DIRECTION ( 'NONE',  ( 0.000000000000000000, 0.000000000000000000, 1.000000000000000000 ) ) ;
#4936 = ITEM_DEFINED_TRANSFORMATION ( 'NONE', 'NONE', #5773,  #285 ) ;
#4937 = ORIENTED_EDGE ( 'NONE', *, *, #14536, .F. ) ;
#4938 = CARTESIAN_POINT ( 'NONE',  ( -69.77438362644001302, 92.67411849586700612, -80.44847958357698303 ) ) ;
#4939 = CARTESIAN_POINT ( 'NONE',  ( -3.018109139697564114, -3.609375000000057732, 2.478742592228960095 ) ) ;
#4940 = EDGE_LOOP ( 'NONE', ( #7288, #9586, #1776, #4397 ) ) ;
#4941 = EDGE_CURVE ( 'NONE', #12703, #6907, #14699, .T. ) ;
#4942 = CARTESIAN_POINT ( 'NONE',  ( -3.705025434593251177, -1.038125000000020393, -1.124966067554165727 ) ) ;
#4943 = DIRECTION ( 'NONE',  ( -1.000000000000000000, 0.000000000000000000, 0.000000000000000000 ) ) ;
#4944 = CARTESIAN_POINT ( 'NONE',  ( -86.77438362644001302, 59.67411849586700612, -152.4984795835769944 ) ) ;
#4945 = CARTESIAN_POINT ( 'NONE',  ( -13.41835358098578723, -12.40000029085423883, -9.367156043074160721 ) ) ;
#4946 = FACE_BOUND ( 'NONE', #6870, .T. ) ;
#4947 = FACE_OUTER_BOUND ( 'NONE', #13990, .T. ) ;
#4948 = FACE_OUTER_BOUND ( 'NONE', #3018, .T. ) ;
#4949 = ORIENTED_EDGE ( 'NONE', *, *, #2887, .T. ) ;
#4950 = DIRECTION ( 'NONE',  ( 0.000000000000000000, 0.000000000000000000, 1.000000000000000000 ) ) ;
#4951 = EDGE_CURVE ( 'NONE', #7246, #14906, #2877, .T. ) ;
#4952 =( LENGTH_UNIT ( ) NAMED_UNIT ( * ) SI_UNIT ( .MILLI., .METRE. ) );
#4953 = ORIENTED_EDGE ( 'NONE', *, *, #2607, .F. ) ;
#4954 = DIRECTION ( 'NONE',  ( 1.000000000000000000, 0.000000000000000000, -0.000000000000000000 ) ) ;
#4955 = CARTESIAN_POINT ( 'NONE',  ( 3.376561219002149894, -3.631875000000035048, -1.025635141340162315 ) ) ;
#4956 = EDGE_LOOP ( 'NONE', ( #10505, #1613, #7114, #14229, #6180 ) ) ;
#4957 = ORIENTED_EDGE ( 'NONE', *, *, #1047, .F. ) ;
#4958 = ADVANCED_FACE ( 'NONE', ( #11295 ), #7670, .T. ) ;
#4959 = EDGE_LOOP ( 'NONE', ( #14967, #11198, #12789, #1296 ) ) ;
#4960 = LINE ( 'NONE', #12805, #1319 ) ;
#4961 = CARTESIAN_POINT ( 'NONE',  ( -80.52077156573417938, 164.3482369917340122, -79.59847958357700293 ) ) ;
#4962 = DIRECTION ( 'NONE',  ( 0.000000000000000000, 0.000000000000000000, -1.000000000000000000 ) ) ;
#4963 = DIRECTION ( 'NONE',  ( -1.000000000000000000, -0.000000000000000000, -0.000000000000000000 ) ) ;
#4964 = CARTESIAN_POINT ( 'NONE',  ( -84.27438362643998460, 65.17411849586700612, -145.2984795835770058 ) ) ;
#4965 = DIRECTION ( 'NONE',  ( 0.000000000000000000, 0.000000000000000000, -1.000000000000000000 ) ) ;
#4966 = CARTESIAN_POINT ( 'NONE',  ( -35.58670980944424400, 5.000000000000001776, 133.4783111191910621 ) ) ;
#4967 = CARTESIAN_POINT ( 'NONE',  ( -0.3378546177656944205, -4.319374999999974207, 3.421346328963575711 ) ) ;
#4968 = DIRECTION ( 'NONE',  ( 0.000000000000000000, 1.000000000000000000, 0.000000000000000000 ) ) ;
#4969 = VERTEX_POINT ( 'NONE', #5332 ) ;
#4970 = CARTESIAN_POINT ( 'NONE',  ( -2.577850803773733546, 4.297149196226267343, 0.000000000000000000 ) ) ;
#4971 = EDGE_CURVE ( 'NONE', #1421, #7439, #13297, .T. ) ;
#4972 = ORIENTED_EDGE ( 'NONE', *, *, #12470, .T. ) ;
#4973 = EDGE_LOOP ( 'NONE', ( #9554, #1629, #539, #2172 ) ) ;
#4974 = VERTEX_POINT ( 'NONE', #1978 ) ;
#4975 = ORIENTED_EDGE ( 'NONE', *, *, #11135, .F. ) ;
#4976 = EDGE_CURVE ( 'NONE', #2643, #7102, #9207, .T. ) ;
#4977 = CARTESIAN_POINT ( 'NONE',  ( 3.463329978863818770, -3.616249999999970210, -0.6879750677194342856 ) ) ;
#4978 = SURFACE_STYLE_FILL_AREA ( #234 ) ;
#4979 = FACE_OUTER_BOUND ( 'NONE', #10369, .T. ) ;
#4980 = EDGE_CURVE ( 'NONE', #13163, #11286, #6581, .T. ) ;
#4981 = DIRECTION ( 'NONE',  ( -1.287488025362404182E-15, -1.000000000000000000, 0.000000000000000000 ) ) ;
#4982 = PLANE ( 'NONE',  #13970 ) ;
#4983 = ADVANCED_FACE ( 'NONE', ( #12616 ), #6727, .T. ) ;
#4984 = DIRECTION ( 'NONE',  ( 0.7933533402912347210, 0.6087614290087212110, 9.715776287805233806E-17 ) ) ;
#4985 = CARTESIAN_POINT ( 'NONE',  ( -53.77438362644000591, 82.17411849586700612, -138.4984795835769944 ) ) ;
#4986 = CARTESIAN_POINT ( 'NONE',  ( 15.50000000000000000, -1.037157890325000054, -22.50000000000000000 ) ) ;
#4987 = ORIENTED_EDGE ( 'NONE', *, *, #11812, .F. ) ;
#4988 = CARTESIAN_POINT ( 'NONE',  ( 0.8000000000000193623, -5.500000000000000888, 9.797174393179008575E-17 ) ) ;
#4989 = ADVANCED_FACE ( 'NONE', ( #6335, #6257 ), #6186, .T. ) ;
#4990 = ORIENTED_EDGE ( 'NONE', *, *, #5738, .T. ) ;
#4991 = CIRCLE ( 'NONE', #2005, 4.500000000000003553 ) ;
#4992 = VERTEX_POINT ( 'NONE', #332 ) ;
#4993 = CARTESIAN_POINT ( 'NONE',  ( 1.553520276525308219, -5.413125000000014175, 2.903814772855817239 ) ) ;
#4994 = ADVANCED_FACE ( 'NONE', ( #6477 ), #3752, .F. ) ;
#4995 = CARTESIAN_POINT ( 'NONE',  ( 3.655516518246672231, 0.09375000000004835021, 2.440638533248514541 ) ) ;
#4996 = EDGE_CURVE ( 'NONE', #4633, #5205, #2378, .T. ) ;
#4997 = CARTESIAN_POINT ( 'NONE',  ( 0.4212773118942713668, -0.7648385623731170924, 4.261548716872522569 ) ) ;
#4998 = CIRCLE ( 'NONE', #1263, 0.5000000000000000000 ) ;
#4999 = DIRECTION ( 'NONE',  ( 0.9961946980917453232, -7.200509705930739692E-17, 0.08715574274766157981 ) ) ;
#5000 = DIRECTION ( 'NONE',  ( 0.000000000000000000, 1.000000000000000000, 0.000000000000000000 ) ) ;
#5001 = DIRECTION ( 'NONE',  ( 0.000000000000000000, 1.000000000000000000, 0.000000000000000000 ) ) ;
#5002 = VECTOR ( 'NONE', #8094, 1000.000000000000000 ) ;
#5003 = CYLINDRICAL_SURFACE ( 'NONE', #9011, 0.6000000000000000888 ) ;
#5004 = FACE_OUTER_BOUND ( 'NONE', #3655, .T. ) ;
#5005 = ORIENTED_EDGE ( 'NONE', *, *, #1762, .T. ) ;
#5006 = CARTESIAN_POINT ( 'NONE',  ( -89.27438362643999881, 65.17411849586700612, -79.59847958357700293 ) ) ;
#5007 = ADVANCED_FACE ( 'NONE', ( #3979 ), #13308, .F. ) ;
#5008 = TOROIDAL_SURFACE ( 'NONE', #13678, 3.299999999999474909, 0.2000000000005234813 ) ;
#5009 = ORIENTED_EDGE ( 'NONE', *, *, #9425, .F. ) ;
#5010 = SHAPE_REPRESENTATION ( 'Pneumatic Cylinder Piston', ( #285 ), #15141 ) ;
#5011 = SURFACE_SIDE_STYLE ('',( #7036 ) ) ;
#5012 = CARTESIAN_POINT ( 'NONE',  ( -2.784563489868539410, -3.375000000000053735, -2.782533402055042071 ) ) ;
#5013 = EDGE_LOOP ( 'NONE', ( #6748, #8591 ) ) ;
#5014 = CIRCLE ( 'NONE', #13187, 4.500000000000003553 ) ;
#5015 = CARTESIAN_POINT ( 'NONE',  ( -3.619583526789921457, -4.546088562373016728, 1.096959227905920597 ) ) ;
#5016 = CARTESIAN_POINT ( 'NONE',  ( 0.001402937982463629916, -1.335000000000034825, 3.832736870811212171 ) ) ;
#5017 = CARTESIAN_POINT ( 'NONE',  ( -3.412320100379302446, -5.286939238114719330, 0.5937987388295963287 ) ) ;
#5018 = VECTOR ( 'NONE', #3426, 1000.000000000000000 ) ;
#5019 = DIRECTION ( 'NONE',  ( 0.000000000000000000, 0.000000000000000000, -1.000000000000000000 ) ) ;
#5020 = DIRECTION ( 'NONE',  ( 0.000000000000000000, 0.000000000000000000, -1.000000000000000000 ) ) ;
#5021 = LINE ( 'NONE', #10761, #5790 ) ;
#5022 = PLANE ( 'NONE',  #10809 ) ;
#5023 = DIRECTION ( 'NONE',  ( -1.000000000000000000, 0.000000000000000000, 0.000000000000000000 ) ) ;
#5024 = AXIS2_PLACEMENT_3D ( 'NONE', #2136, #5797, #10503 ) ;
#5025 = ORIENTED_EDGE ( 'NONE', *, *, #7265, .T. ) ;
#5026 = CARTESIAN_POINT ( 'NONE',  ( 101.9614256548736364, 5.000000000000000000, 101.9614256548729259 ) ) ;
#5027 = EDGE_LOOP ( 'NONE', ( #14176, #14800, #13505, #14398 ) ) ;
#5028 = AXIS2_PLACEMENT_3D ( 'NONE', #201, #8506, #11925 ) ;
#5029 = CARTESIAN_POINT ( 'NONE',  ( 21.98164641901421135, 12.49999970914576153, -8.775548064764198131 ) ) ;
#5030 = CARTESIAN_POINT ( 'NONE',  ( 2.928286698324767734, -3.678750000000110987, -1.958188979435659283 ) ) ;
#5031 = ORIENTED_EDGE ( 'NONE', *, *, #12900, .F. ) ;
#5032 = EDGE_LOOP ( 'NONE', ( #7719, #10524, #5905, #12636 ) ) ;
#5033 = VERTEX_POINT ( 'NONE', #7570 ) ;
#5034 = CIRCLE ( 'NONE', #11720, 0.2000000000000057288 ) ;
#5035 = DIRECTION ( 'NONE',  ( -1.000000000000000000, 0.000000000000000000, 0.000000000000000000 ) ) ;
#5036 = AXIS2_PLACEMENT_3D ( 'NONE', #7078, #11490, #9153 ) ;
#5037 = DIRECTION ( 'NONE',  ( -1.000000000000000000, 0.000000000000000000, 0.000000000000000000 ) ) ;
#5038 = EDGE_CURVE ( 'NONE', #11568, #7541, #2668, .T. ) ;
#5039 = CARTESIAN_POINT ( 'NONE',  ( -56.85838362644099675, 99.17411849586700612, -147.9984795835769944 ) ) ;
#5040 = CARTESIAN_POINT ( 'NONE',  ( -4.287904177287694907, -0.4995676945082599407, -0.3292842791088227417 ) ) ;
#5041 = CARTESIAN_POINT ( 'NONE',  ( 14.66242688423474050, -0.3152598339554796292, -21.54019739087904384 ) ) ;
#5042 = EDGE_CURVE ( 'NONE', #181, #4720, #13457, .T. ) ;
#5043 = CARTESIAN_POINT ( 'NONE',  ( -30.00000000000000000, -5.000000000000000000, 27.00000000000000000 ) ) ;
#5044 = EDGE_LOOP ( 'NONE', ( #12380, #6589 ) ) ;
#5045 = CARTESIAN_POINT ( 'NONE',  ( -69.77438362644001302, 82.17411849586700612, -79.49847958357700861 ) ) ;
#5046 = AXIS2_PLACEMENT_3D ( 'NONE', #4307, #8024, #9034 ) ;
#5047 = CIRCLE ( 'NONE', #2059, 1.000000000000000888 ) ;
#5048 = ORIENTED_EDGE ( 'NONE', *, *, #2193, .F. ) ;
#5049 = EDGE_LOOP ( 'NONE', ( #7563, #7223, #10548, #4033 ) ) ;
#5050 = ORIENTED_EDGE ( 'NONE', *, *, #14827, .T. ) ;
#5051 = EDGE_LOOP ( 'NONE', ( #4567, #11642, #3357, #15217 ) ) ;
#5052 = AXIS2_PLACEMENT_3D ( 'NONE', #8698, #1567, #316 ) ;
#5053 = DIRECTION ( 'NONE',  ( -1.000000000000000000, 0.000000000000000000, 0.000000000000000000 ) ) ;
#5054 = CARTESIAN_POINT ( 'NONE',  ( 1.779210140229128934, -1.756874999999983755, -3.331607052712222572 ) ) ;
#5055 = CARTESIAN_POINT ( 'NONE',  ( 3.775473633219732505, -4.031249999999629630, -0.7524242524445519109 ) ) ;
#5056 = AXIS2_PLACEMENT_3D ( 'NONE', #9947, #13462, #14530 ) ;
#5057 = FACE_BOUND ( 'NONE', #6797, .T. ) ;
#5058 = EDGE_CURVE ( 'NONE', #7838, #3706, #3909, .T. ) ;
#5059 = AXIS2_PLACEMENT_3D ( 'NONE', #9760, #13276, #7224 ) ;
#5060 = DIRECTION ( 'NONE',  ( -1.000000000000000000, 0.000000000000000000, 0.000000000000000000 ) ) ;
#5061 = LINE ( 'NONE', #309, #13828 ) ;
#5062 = CARTESIAN_POINT ( 'NONE',  ( -59.02799568714584666, 60.67411849586701322, -73.34256232478206528 ) ) ;
#5063 = CYLINDRICAL_SURFACE ( 'NONE', #2359, 4.500000000000003553 ) ;
#5064 = LINE ( 'NONE', #7320, #1134 ) ;
#5065 = EDGE_CURVE ( 'NONE', #13986, #2062, #7596, .T. ) ;
#5066 = DIRECTION ( 'NONE',  ( -0.000000000000000000, -0.000000000000000000, -1.000000000000000000 ) ) ;
#5067 = EDGE_LOOP ( 'NONE', ( #10922, #10890, #15099, #1930 ) ) ;
#5068 = DIRECTION ( 'NONE',  ( 0.000000000000000000, 0.000000000000000000, -1.000000000000000000 ) ) ;
#5069 = ORIENTED_EDGE ( 'NONE', *, *, #2419, .T. ) ;
#5070 = ORIENTED_EDGE ( 'NONE', *, *, #12932, .T. ) ;
#5071 = CARTESIAN_POINT ( 'NONE',  ( -0.9391448502757393513, -5.881874999999767262, -3.091762488354312222 ) ) ;
#5072 = AXIS2_PLACEMENT_3D ( 'NONE', #9662, #8513, #12093 ) ;
#5073 = VECTOR ( 'NONE', #7450, 1000.000000000000000 ) ;
#5074 = EDGE_CURVE ( 'NONE', #6450, #4436, #5078, .T. ) ;
#5075 = DIRECTION ( 'NONE',  ( -1.000000000000000000, -1.783664229908549233E-15, 0.000000000000000000 ) ) ;
#5076 = B_SPLINE_CURVE_WITH_KNOTS ( 'NONE', 3,
 ( #4237, #14780, #13631, #663, #13478, #7734, #2843, #511, #12462, #8963, #1826, #5416, #10117, #13701 ),
 .UNSPECIFIED., .F., .F.,
 ( 4, 2, 2, 2, 2, 2, 4 ),
 ( 0.004061142180336881069, 0.005409079593014973729, 0.006083048299354019625, 0.006757017005693066389, 0.008104954418371158181, 0.008778923124710204945, 0.009452891831049249974 ),
 .UNSPECIFIED. ) ;
#5077 = CARTESIAN_POINT ( 'NONE',  ( 4.074635740569324760, -0.9523385623730679095, 1.234421966825711481 ) ) ;
#5078 = LINE ( 'NONE', #9870, #408 ) ;
#5079 = CARTESIAN_POINT ( 'NONE',  ( -57.02438362643999170, 65.17411849586700612, -182.2484795835770228 ) ) ;
#5080 = ADVANCED_FACE ( 'NONE', ( #12369 ), #494, .T. ) ;
#5081 = CARTESIAN_POINT ( 'NONE',  ( -61.42438362644001160, 82.17411849586700612, -80.14847958357698587 ) ) ;
#5082 = CARTESIAN_POINT ( 'NONE',  ( -52.77438362644100067, 99.17411849586700612, -150.4984795835770228 ) ) ;
#5083 = CARTESIAN_POINT ( 'NONE',  ( -6.714472293954754534, 11.99999970914575975, 37.72291661448763733 ) ) ;
#5084 = AXIS2_PLACEMENT_3D ( 'NONE', #8584, #6356, #5179 ) ;
#5085 = EDGE_CURVE ( 'NONE', #9494, #13360, #8817, .T. ) ;
#5086 = FACE_OUTER_BOUND ( 'NONE', #14690, .T. ) ;
#5087 = EDGE_CURVE ( 'NONE', #12014, #13910, #3342, .T. ) ;
#5088 = ORIENTED_EDGE ( 'NONE', *, *, #6429, .F. ) ;
#5089 = LINE ( 'NONE', #14533, #4379 ) ;
#5090 = VERTEX_POINT ( 'NONE', #7333 ) ;
#5091 = SURFACE_STYLE_USAGE ( .BOTH. , #10981 ) ;
#5092 = EDGE_CURVE ( 'NONE', #6469, #3787, #2891, .T. ) ;
#5093 = CARTESIAN_POINT ( 'NONE',  ( -1.920019182618211584, -2.328124999999937383, -3.594387849940205104 ) ) ;
#5094 = ORIENTED_EDGE ( 'NONE', *, *, #9993, .F. ) ;
#5095 = AXIS2_PLACEMENT_3D ( 'NONE', #4011, #1913, #11300 ) ;
#5096 = VECTOR ( 'NONE', #14360, 1000.000000000000000 ) ;
#5097 = CARTESIAN_POINT ( 'NONE',  ( 2.619318502887032718, -5.124213562373151731, -2.621246189942336713 ) ) ;
#5098 = AXIS2_PLACEMENT_3D ( 'NONE', #10876, #8846, #9141 ) ;
#5099 = VECTOR ( 'NONE', #8622, 1000.000000000000000 ) ;
#5100 = CARTESIAN_POINT ( 'NONE',  ( 3.915012698312653860, -0.5693749999999865308, 0.3866328316385073127 ) ) ;
#5101 = ADVANCED_FACE ( 'NONE', ( #419, #12063 ), #14599, .T. ) ;
#5102 = CARTESIAN_POINT ( 'NONE',  ( 15.50000000000000000, -0.2038245569916604938, 23.94337567297399971 ) ) ;
#5103 = CARTESIAN_POINT ( 'NONE',  ( -6.714472293954755422, -12.00000029085427578, 37.72291661448763733 ) ) ;
#5104 = FACE_OUTER_BOUND ( 'NONE', #13093, .T. ) ;
#5105 = DIRECTION ( 'NONE',  ( -0.000000000000000000, -0.000000000000000000, -1.000000000000000000 ) ) ;
#5106 = DIRECTION ( 'NONE',  ( -1.000000000000000000, 0.000000000000000000, -0.000000000000000000 ) ) ;
#5107 = CYLINDRICAL_SURFACE ( 'NONE', #5123, 1.785937500000001066 ) ;
#5108 = VECTOR ( 'NONE', #13007, 1000.000000000000114 ) ;
#5109 = DIRECTION ( 'NONE',  ( 0.000000000000000000, 1.000000000000000000, 0.000000000000000000 ) ) ;
#5110 = CARTESIAN_POINT ( 'NONE',  ( -52.77438362643999881, 62.81621999649657084, -147.9984795835769944 ) ) ;
#5111 = VECTOR ( 'NONE', #14145, 1000.000000000000114 ) ;
#5112 = ORIENTED_EDGE ( 'NONE', *, *, #7230, .F. ) ;
#5113 = AXIS2_PLACEMENT_3D ( 'NONE', #12029, #5273, #7299 ) ;
#5114 = ORIENTED_EDGE ( 'NONE', *, *, #12919, .T. ) ;
#5115 = EDGE_LOOP ( 'NONE', ( #3863, #11469, #10125, #15117, #14121 ) ) ;
#5116 = CARTESIAN_POINT ( 'NONE',  ( -69.77438362644001302, 82.17411849586700612, -150.4984795835769944 ) ) ;
#5117 = CARTESIAN_POINT ( 'NONE',  ( 2.337649614532406162, -2.444375000000051479, 2.849939602875970035 ) ) ;
#5118 = EDGE_LOOP ( 'NONE', ( #2701, #1897 ) ) ;
#5119 = ORIENTED_EDGE ( 'NONE', *, *, #7660, .F. ) ;
#5120 = CIRCLE ( 'NONE', #10299, 17.00000000000000000 ) ;
#5121 = DIRECTION ( 'NONE',  ( -0.8660254037844387076, -0.4999999999999998890, 0.000000000000000000 ) ) ;
#5122 = CIRCLE ( 'NONE', #11554, 0.1999999999999987899 ) ;
#5123 = AXIS2_PLACEMENT_3D ( 'NONE', #13332, #2844, #1371 ) ;
#5124 = FACE_OUTER_BOUND ( 'NONE', #9103, .T. ) ;
#5125 = PLANE ( 'NONE',  #15201 ) ;
#5126 = DIRECTION ( 'NONE',  ( 0.000000000000000000, -0.000000000000000000, 1.000000000000000000 ) ) ;
#5127 = DIRECTION ( 'NONE',  ( 1.000000000000000000, -0.000000000000000000, 0.000000000000000000 ) ) ;
#5128 = DIRECTION ( 'NONE',  ( 0.000000000000000000, 0.000000000000000000, 1.000000000000000000 ) ) ;
#5129 = ORIENTED_EDGE ( 'NONE', *, *, #13140, .F. ) ;
#5130 = DIRECTION ( 'NONE',  ( 0.000000000000000000, 1.000000000000000000, 0.000000000000000000 ) ) ;
#5131 = AXIS2_PLACEMENT_3D ( 'NONE', #1828, #14925, #812 ) ;
#5132 = ORIENTED_EDGE ( 'NONE', *, *, #4980, .T. ) ;
#5133 = AXIS2_PLACEMENT_3D ( 'NONE', #8377, #10694, #2318 ) ;
#5134 = ORIENTED_EDGE ( 'NONE', *, *, #3952, .T. ) ;
#5135 = ORIENTED_EDGE ( 'NONE', *, *, #3354, .F. ) ;
#5136 = ORIENTED_EDGE ( 'NONE', *, *, #9618, .F. ) ;
#5137 = EDGE_LOOP ( 'NONE', ( #8534, #8204, #6115, #15095, #1060 ) ) ;
#5138 = CARTESIAN_POINT ( 'NONE',  ( -53.70938362644000819, 81.46011849586699327, -83.44847958357698303 ) ) ;
#5139 = CARTESIAN_POINT ( 'NONE',  ( -2.629016928070645243, -2.210000000000078568, 2.627652665972809665 ) ) ;
#5140 = EDGE_CURVE ( 'NONE', #11281, #4564, #7489, .T. ) ;
#5141 = VECTOR ( 'NONE', #10350, 1000.000000000000000 ) ;
#5142 = CARTESIAN_POINT ( 'NONE',  ( 0.7730394778201963302, -3.218749999999914735, -3.881000975522858720 ) ) ;
#5143 = DIRECTION ( 'NONE',  ( 0.8660254037844482555, 0.000000000000000000, 0.4999999999999831801 ) ) ;
#5144 = DIRECTION ( 'NONE',  ( -0.000000000000000000, 0.000000000000000000, 1.000000000000000000 ) ) ;
#5145 = AXIS2_PLACEMENT_3D ( 'NONE', #4178, #3307, #596 ) ;
#5146 = FACE_OUTER_BOUND ( 'NONE', #12570, .T. ) ;
#5147 = CARTESIAN_POINT ( 'NONE',  ( 15.50000000000000000, -5.000000000000000000, -26.00000000000000000 ) ) ;
#5148 = CARTESIAN_POINT ( 'NONE',  ( -50.73238362644099197, 100.3530677455522238, -147.9984795835769944 ) ) ;
#5149 = CYLINDRICAL_SURFACE ( 'NONE', #10737, 4.000000000000000000 ) ;
#5150 = ORIENTED_EDGE ( 'NONE', *, *, #10541, .F. ) ;
#5151 = CARTESIAN_POINT ( 'NONE',  ( -73.76311196519618818, 67.29799558322736175, -83.44847958357698303 ) ) ;
#5152 = ORIENTED_EDGE ( 'NONE', *, *, #8668, .T. ) ;
#5153 = EDGE_LOOP ( 'NONE', ( #14177, #6120 ) ) ;
#5154 = ORIENTED_EDGE ( 'NONE', *, *, #3349, .F. ) ;
#5155 = UNCERTAINTY_MEASURE_WITH_UNIT (LENGTH_MEASURE( 1.000000000000000082E-05 ), #11839, 'distance_accuracy_value', 'NONE');
#5156 = CARTESIAN_POINT ( 'NONE',  ( 1.804507757947518609, -5.741250000000162501, -2.702832914148806776 ) ) ;
#5157 = ADVANCED_FACE ( 'NONE', ( #11416, #14759 ), #1882, .T. ) ;
#5158 = VECTOR ( 'NONE', #13544, 1000.000000000000000 ) ;
#5159 = CARTESIAN_POINT ( 'NONE',  ( -44.58670980944423690, 5.000000000000000000, 137.5095611191910621 ) ) ;
#5160 = CARTESIAN_POINT ( 'NONE',  ( -1.266249875242109413, -5.272499999999733511, 3.060236832100306614 ) ) ;
#5161 = CARTESIAN_POINT ( 'NONE',  ( 16.75000000000000000, -2.500000000000000000, 23.22168783648699986 ) ) ;
#5162 = DIRECTION ( 'NONE',  ( 0.000000000000000000, -1.000000000000000000, 0.000000000000000000 ) ) ;
#5163 = LINE ( 'NONE', #9872, #8340 ) ;
#5164 = ADVANCED_BREP_SHAPE_REPRESENTATION ( '', ( #442, #285 ), #8480 ) ;
#5165 = FACE_OUTER_BOUND ( 'NONE', #4738, .T. ) ;
#5166 = DIRECTION ( 'NONE',  ( 0.000000000000000000, 0.000000000000000000, -1.000000000000000000 ) ) ;
#5167 = CARTESIAN_POINT ( 'NONE',  ( -2.093999815491831562, 9.499999999999998224, 2.703148537761814673E-16 ) ) ;
#5168 = VERTEX_POINT ( 'NONE', #13679 ) ;
#5169 = CARTESIAN_POINT ( 'NONE',  ( 14.25000000000000000, -2.500000000000000000, -23.22168783648699986 ) ) ;
#5170 = EDGE_CURVE ( 'NONE', #7524, #13652, #8087, .T. ) ;
#5171 = ORIENTED_EDGE ( 'NONE', *, *, #12867, .F. ) ;
#5172 = CARTESIAN_POINT ( 'NONE',  ( 3.414669715040141273, -2.093749999999965805, -2.280302418758094252 ) ) ;
#5173 = ORIENTED_EDGE ( 'NONE', *, *, #15106, .T. ) ;
#5174 = EDGE_CURVE ( 'NONE', #11015, #12263, #12064, .T. ) ;
#5175 = AXIS2_PLACEMENT_3D ( 'NONE', #5525, #9218, #13882 ) ;
#5176 = DIRECTION ( 'NONE',  ( -1.000000000000000000, 0.000000000000000000, -0.000000000000000000 ) ) ;
#5177 = CARTESIAN_POINT ( 'NONE',  ( -80.52077156573417938, 164.3482369917340122, -73.34256232478206528 ) ) ;
#5178 = LINE ( 'NONE', #5103, #12465 ) ;
#5179 = DIRECTION ( 'NONE',  ( -1.000000000000000000, 0.000000000000000000, 0.000000000000000000 ) ) ;
#5180 = EDGE_CURVE ( 'NONE', #4176, #2932, #10325, .T. ) ;
#5181 = DIRECTION ( 'NONE',  ( 0.000000000000000000, -1.000000000000000000, 0.000000000000000000 ) ) ;
#5182 = DIRECTION ( 'NONE',  ( -0.9961946980917452121, 7.200509705930737227E-17, -0.08715574274766155205 ) ) ;
#5183 = CARTESIAN_POINT ( 'NONE',  ( -42.77438362644000591, 65.17411849586700612, -79.59847958357700293 ) ) ;
#5184 = CARTESIAN_POINT ( 'NONE',  ( -15.50000000000000000, -2.500000000000000000, 21.05662432702600029 ) ) ;
#5185 = CARTESIAN_POINT ( 'NONE',  ( 37.35543536254874653, -19.31989681812820692, 0.000000000000000000 ) ) ;
#5186 = AXIS2_PLACEMENT_3D ( 'NONE', #4554, #9277, #678 ) ;
#5187 = ORIENTED_EDGE ( 'NONE', *, *, #6346, .T. ) ;
#5188 = ADVANCED_FACE ( 'NONE', ( #12660 ), #6854, .T. ) ;
#5189 = ORIENTED_EDGE ( 'NONE', *, *, #14175, .F. ) ;
#5190 = CARTESIAN_POINT ( 'NONE',  ( 15.50000000000000000, -1.037157890325000054, -22.50000000000000000 ) ) ;
#5191 = CARTESIAN_POINT ( 'NONE',  ( -1.113040416940732857, -1.288124999999980425, 3.674042195187707804 ) ) ;
#5192 = ORIENTED_EDGE ( 'NONE', *, *, #4798, .F. ) ;
#5193 = EDGE_CURVE ( 'NONE', #6231, #3959, #863, .T. ) ;
#5194 = EDGE_CURVE ( 'NONE', #9136, #14122, #4628, .T. ) ;
#5195 = DIRECTION ( 'NONE',  ( 0.3469356515732570645, 0.9378889346118971515, 0.000000000000000000 ) ) ;
#5196 = CARTESIAN_POINT ( 'NONE',  ( 0.3693243909029986227, -5.159404925397325314, -3.617482621258250486 ) ) ;
#5197 = DIRECTION ( 'NONE',  ( 0.000000000000000000, -0.000000000000000000, 1.000000000000000000 ) ) ;
#5198 = CARTESIAN_POINT ( 'NONE',  ( -48.27438362644000591, 99.17411849586700612, -152.4984795835769944 ) ) ;
#5199 = SURFACE_SIDE_STYLE ('',( #5504 ) ) ;
#5200 = CARTESIAN_POINT ( 'NONE',  ( -14.25000000000000178, -0.2714405302574905976, -22.98746066354537732 ) ) ;
#5201 = CARTESIAN_POINT ( 'NONE',  ( -62.27438362644000591, 89.17411849586700612, -57.99847958357699440 ) ) ;
#5202 = EDGE_LOOP ( 'NONE', ( #15335, #2969 ) ) ;
#5203 = DIRECTION ( 'NONE',  ( -0.000000000000000000, 1.000000000000000000, -0.000000000000000000 ) ) ;
#5204 = ORIENTED_EDGE ( 'NONE', *, *, #2584, .F. ) ;
#5205 = VERTEX_POINT ( 'NONE', #5621 ) ;
#5206 = ORIENTED_EDGE ( 'NONE', *, *, #7265, .F. ) ;
#5207 = ORIENTED_EDGE ( 'NONE', *, *, #10009, .F. ) ;
#5208 = EDGE_LOOP ( 'NONE', ( #37, #12469, #14824, #11249 ) ) ;
#5209 = DIRECTION ( 'NONE',  ( 0.000000000000000000, -1.000000000000000000, 0.000000000000000000 ) ) ;
#5210 = CARTESIAN_POINT ( 'NONE',  ( 1.412068586280907923, -2.397499999999971099, 3.411535633775557574 ) ) ;
#5211 = CARTESIAN_POINT ( 'NONE',  ( -2.165165973034034685, -3.656250000000003997, 3.242962682996374912 ) ) ;
#5212 = DIRECTION ( 'NONE',  ( 1.000000000000000000, 0.000000000000000000, 0.000000000000000000 ) ) ;
#5213 = CARTESIAN_POINT ( 'NONE',  ( -52.77438362643999881, 62.81621999649657084, -150.4984795835770228 ) ) ;
#5214 = CARTESIAN_POINT ( 'NONE',  ( -52.77438362644000591, 82.17411849586700612, -3.496191900462991775 ) ) ;
#5215 = LINE ( 'NONE', #1329, #8015 ) ;
#5216 = CARTESIAN_POINT ( 'NONE',  ( -62.02799568714584666, 103.6741184958669919, -152.4984795835769944 ) ) ;
#5217 = DIRECTION ( 'NONE',  ( 1.000000000000000000, -1.287488025362404182E-15, 0.000000000000000000 ) ) ;
#5218 = PRODUCT ( 'BR-Y-114', 'BR-Y-114', '', ( #12688 ) ) ;
#5219 = DIRECTION ( 'NONE',  ( -1.000000000000000000, 0.000000000000000000, 0.000000000000000000 ) ) ;
#5220 = VERTEX_POINT ( 'NONE', #10096 ) ;
#5221 = LINE ( 'NONE', #2892, #13716 ) ;
#5222 = ORIENTED_EDGE ( 'NONE', *, *, #12631, .F. ) ;
#5223 = ORIENTED_EDGE ( 'NONE', *, *, #14711, .T. ) ;
#5224 = CARTESIAN_POINT ( 'NONE',  ( -2.589953986283602294, -4.975625000000236220, -2.126619835350849641 ) ) ;
#5225 = CARTESIAN_POINT ( 'NONE',  ( 57.41329019055577021, 0.000000000000000000, 127.7236236191910734 ) ) ;
#5226 = DIRECTION ( 'NONE',  ( -1.000000000000000000, 0.000000000000000000, 0.000000000000000000 ) ) ;
#5227 = CARTESIAN_POINT ( 'NONE',  ( -82.52438362644100778, 99.17411849586700612, -149.9984795835770228 ) ) ;
#5228 = FACE_OUTER_BOUND ( 'NONE', #4076, .T. ) ;
#5229 = CARTESIAN_POINT ( 'NONE',  ( -86.77438362643999881, 62.81621999649657084, -147.9984795835769944 ) ) ;
#5230 = FACE_BOUND ( 'NONE', #12214, .T. ) ;
#5231 = ADVANCED_FACE ( 'NONE', ( #783 ), #6639, .F. ) ;
#5232 = AXIS2_PLACEMENT_3D ( 'NONE', #12856, #13099, #9274 ) ;
#5233 = DIRECTION ( 'NONE',  ( -1.000000000000000000, 0.000000000000000000, -0.000000000000000000 ) ) ;
#5234 = VERTEX_POINT ( 'NONE', #11350 ) ;
#5235 = LINE ( 'NONE', #4375, #7122 ) ;
#5236 = ADVANCED_FACE ( 'NONE', ( #2106 ), #9561, .T. ) ;
#5237 = VERTEX_POINT ( 'NONE', #5311 ) ;
#5238 = CIRCLE ( 'NONE', #4487, 4.401041666666736241 ) ;
#5239 = DIRECTION ( 'NONE',  ( -0.000000000000000000, 0.000000000000000000, 1.000000000000000000 ) ) ;
#5240 = CARTESIAN_POINT ( 'NONE',  ( 0.3952026422296860964, -2.765624999999906741, 3.997656568947202338 ) ) ;
#5241 = ORIENTED_EDGE ( 'NONE', *, *, #14757, .T. ) ;
#5242 = CIRCLE ( 'NONE', #12924, 17.00000000000000000 ) ;
#5243 = CARTESIAN_POINT ( 'NONE',  ( -69.77438362644001302, 82.17411849586700612, -81.84847958357698872 ) ) ;
#5244 = LINE ( 'NONE', #8580, #1375 ) ;
#5245 = CARTESIAN_POINT ( 'NONE',  ( 0.8000000000000113687, 9.500000000000000000, 9.797174393178965434E-17 ) ) ;
#5246 = EDGE_CURVE ( 'NONE', #11629, #13653, #4213, .T. ) ;
#5247 = AXIS2_PLACEMENT_3D ( 'NONE', #6874, #1973, #12759 ) ;
#5248 = DIRECTION ( 'NONE',  ( 0.000000000000000000, 1.000000000000000000, 0.000000000000000000 ) ) ;
#5249 = PLANE ( 'NONE',  #3292 ) ;
#5250 = CARTESIAN_POINT ( 'NONE',  ( -9.797174393178965434E-17, 9.500000000000000000, 0.000000000000000000 ) ) ;
#5251 = DIRECTION ( 'NONE',  ( 0.000000000000000000, 1.000000000000000000, 0.000000000000000000 ) ) ;
#5252 = DIRECTION ( 'NONE',  ( 2.551930889570659960E-15, -1.000000000000000000, -0.000000000000000000 ) ) ;
#5253 = VECTOR ( 'NONE', #8335, 1000.000000000000000 ) ;
#5254 = VERTEX_POINT ( 'NONE', #2976 ) ;
#5255 = AXIS2_PLACEMENT_3D ( 'NONE', #7738, #4006, #9040 ) ;
#5256 = CARTESIAN_POINT ( 'NONE',  ( 0.000000000000000000, 0.000000000000000000, 0.000000000000000000 ) ) ;
#5257 = EDGE_LOOP ( 'NONE', ( #1971, #1499, #2742, #4008, #8494, #14377, #8135, #8761, #9932, #8099, #13872, #7640, #14885, #5475, #2595, #432, #7673, #11492, #4342, #10764, #14554, #14191, #8156, #193 ) ) ;
#5258 = CARTESIAN_POINT ( 'NONE',  ( -73.64736697264743270, 75.17411849586699191, -57.99847958357699440 ) ) ;
#5259 = CARTESIAN_POINT ( 'NONE',  ( -2.976231983981254992, -1.194374999999927578, 2.444352914378568276 ) ) ;
#5260 = VERTEX_POINT ( 'NONE', #7713 ) ;
#5261 = VECTOR ( 'NONE', #6778, 1000.000000000000000 ) ;
#5262 = EDGE_CURVE ( 'NONE', #12075, #6505, #13831, .T. ) ;
#5263 = B_SPLINE_CURVE_WITH_KNOTS ( 'NONE', 3,
 ( #3347, #9161, #4592, #13899 ),
 .UNSPECIFIED., .F., .F.,
 ( 4, 4 ),
 ( 0.002598307151460991539, 0.005196383362814307842 ),
 .UNSPECIFIED. ) ;
#5264 = ADVANCED_FACE ( 'NONE', ( #715, #7788 ), #1958, .T. ) ;
#5265 = DIRECTION ( 'NONE',  ( -1.000000000000000000, 0.000000000000000000, 0.000000000000000000 ) ) ;
#5266 = CIRCLE ( 'NONE', #13185, 0.2000000000005226763 ) ;
#5267 = CARTESIAN_POINT ( 'NONE',  ( -52.77438362643999881, 65.17411849586700612, -145.4984795835769944 ) ) ;
#5268 = AXIS2_PLACEMENT_3D ( 'NONE', #14152, #2283, #11448 ) ;
#5269 = EDGE_CURVE ( 'NONE', #6473, #12431, #14896, .T. ) ;
#5270 = CARTESIAN_POINT ( 'NONE',  ( -86.77438362643999881, 67.53201699523744139, -150.4984795835770228 ) ) ;
#5271 = CARTESIAN_POINT ( 'NONE',  ( -35.58670980944424400, 2.488961461112888074, 97.50956111919106206 ) ) ;
#5272 =( NAMED_UNIT ( * ) PLANE_ANGLE_UNIT ( ) SI_UNIT ( $, .RADIAN. ) );
#5273 = DIRECTION ( 'NONE',  ( 0.000000000000000000, -0.000000000000000000, 1.000000000000000000 ) ) ;
#5274 = EDGE_CURVE ( 'NONE', #8682, #11015, #2019, .T. ) ;
#5275 = CARTESIAN_POINT ( 'NONE',  ( -15.50000000000000000, -1.037157890325000054, 22.50000000000000000 ) ) ;
#5276 = PRESENTATION_LAYER_ASSIGNMENT (  '', '', ( #4527 ) ) ;
#5277 = EDGE_CURVE ( 'NONE', #13838, #13566, #6707, .T. ) ;
#5278 = VERTEX_POINT ( 'NONE', #5769 ) ;
#5279 = CARTESIAN_POINT ( 'NONE',  ( -14.25000000000000000, -0.2038245569916330158, 23.22168783648699986 ) ) ;
#5280 = VERTEX_POINT ( 'NONE', #3662 ) ;
#5281 = ORIENTED_EDGE ( 'NONE', *, *, #4215, .F. ) ;
#5282 = EDGE_LOOP ( 'NONE', ( #12280, #13003, #5305, #1772 ) ) ;
#5283 = ORIENTED_EDGE ( 'NONE', *, *, #4338, .F. ) ;
#5284 = AXIS2_PLACEMENT_3D ( 'NONE', #11254, #4123, #3183 ) ;
#5285 = ORIENTED_EDGE ( 'NONE', *, *, #6219, .F. ) ;
#5286 = DIRECTION ( 'NONE',  ( -0.9961946980917453232, 3.779777825264101491E-17, -0.08715574274766164919 ) ) ;
#5287 = EDGE_CURVE ( 'NONE', #9156, #12927, #13861, .T. ) ;
#5288 = CARTESIAN_POINT ( 'NONE',  ( 3.667419683216786908, -2.585000000000003517, 0.0009491222189788412963 ) ) ;
#5289 = VECTOR ( 'NONE', #12825, 1000.000000000000000 ) ;
#5290 =( LENGTH_UNIT ( ) NAMED_UNIT ( * ) SI_UNIT ( .MILLI., .METRE. ) );
#5291 = CARTESIAN_POINT ( 'NONE',  ( 2.712400463490634017, -4.125000000000058620, -2.714386550172725787 ) ) ;
#5292 = CYLINDRICAL_SURFACE ( 'NONE', #1564, 1.999999999999986233 ) ;
#5293 = EDGE_CURVE ( 'NONE', #2023, #10086, #14056, .T. ) ;
#5294 = CARTESIAN_POINT ( 'NONE',  ( -9.797174393178927223E-17, 9.500000000000000000, 0.000000000000000000 ) ) ;
#5295 = CARTESIAN_POINT ( 'NONE',  ( 11.95279236174586224, -8.891480818932939924E-16, 59.43248740176664313 ) ) ;
#5296 = CARTESIAN_POINT ( 'NONE',  ( -4.264150341155778179, -0.5211359837986738741, 0.5700929974395811950 ) ) ;
#5297 = LINE ( 'NONE', #4049, #5099 ) ;
#5298 = TOROIDAL_SURFACE ( 'NONE', #5046, 3.299999999999470024, 0.2000000000005275058 ) ;
#5299 = DIRECTION ( 'NONE',  ( 0.000000000000000000, 0.000000000000000000, -1.000000000000000000 ) ) ;
#5300 = DIRECTION ( 'NONE',  ( 0.000000000000000000, 0.000000000000000000, -1.000000000000000000 ) ) ;
#5301 = ORIENTED_EDGE ( 'NONE', *, *, #9833, .T. ) ;
#5302 = CARTESIAN_POINT ( 'NONE',  ( -4.330127018922192761, -1.133719399746323553E-14, 1.499999999999998002 ) ) ;
#5303 = ORIENTED_EDGE ( 'NONE', *, *, #2147, .F. ) ;
#5304 = AXIS2_PLACEMENT_3D ( 'NONE', #3336, #1400, #4968 ) ;
#5305 = ORIENTED_EDGE ( 'NONE', *, *, #12556, .F. ) ;
#5306 = VERTEX_POINT ( 'NONE', #940 ) ;
#5307 = UNCERTAINTY_MEASURE_WITH_UNIT (LENGTH_MEASURE( 1.000000000000000082E-05 ), #7134, 'distance_accuracy_value', 'NONE');
#5308 = CARTESIAN_POINT ( 'NONE',  ( -76.26311196519618818, 67.29799558322736175, -83.44847958357698303 ) ) ;
#5309 = AXIS2_PLACEMENT_3D ( 'NONE', #5856, #15128, #6011 ) ;
#5310 = AXIS2_PLACEMENT_3D ( 'NONE', #10065, #14798, #6677 ) ;
#5311 = CARTESIAN_POINT ( 'NONE',  ( -102.2743836264399988, 65.17411849586700612, -152.4984795835769944 ) ) ;
#5312 = DIRECTION ( 'NONE',  ( -0.000000000000000000, -0.000000000000000000, 1.000000000000000000 ) ) ;
#5313 = DIRECTION ( 'NONE',  ( 1.000000000000000000, 0.000000000000000000, 0.000000000000000000 ) ) ;
#5314 = CARTESIAN_POINT ( 'NONE',  ( -88.81638362644100937, 97.99516924618178848, -147.9984795835769944 ) ) ;
#5315 = CARTESIAN_POINT ( 'NONE',  ( 0.5699749950174962665, -0.4995676945082574427, 4.018060920292908733 ) ) ;
#5316 = CARTESIAN_POINT ( 'NONE',  ( -0.9755776780686565841, -4.881874999999863185, -3.218989981404408951 ) ) ;
#5317 = EDGE_LOOP ( 'NONE', ( #12865, #8389, #13803, #7762 ) ) ;
#5318 = CARTESIAN_POINT ( 'NONE',  ( -86.77438362644100778, 96.81621999649657084, -150.4984795835770228 ) ) ;
#5319 = CIRCLE ( 'NONE', #14708, 16.06499999999999773 ) ;
#5320 = ORIENTED_EDGE ( 'NONE', *, *, #13699, .F. ) ;
#5321 = CARTESIAN_POINT ( 'NONE',  ( -0.7834809220335302582, -2.718750000000123013, 3.946322201046845279 ) ) ;
#5322 = ORIENTED_EDGE ( 'NONE', *, *, #5269, .T. ) ;
#5323 = CLOSED_SHELL ( 'NONE', ( #12663, #8273, #11613, #1742, #4758, #8459, #11305, #9303, #12656, #4031, #6117, #7905, #15289, #1281 ) ) ;
#5324 = CARTESIAN_POINT ( 'NONE',  ( -52.77438362643999881, 65.17411849586700612, -149.9984795835770228 ) ) ;
#5325 = AXIS2_PLACEMENT_3D ( 'NONE', #7898, #13647, #15019 ) ;
#5326 = EDGE_CURVE ( 'NONE', #10086, #4564, #7326, .T. ) ;
#5327 = AXIS2_PLACEMENT_3D ( 'NONE', #903, #10433, #9356 ) ;
#5328 = PLANE ( 'NONE',  #13542 ) ;
#5329 = CARTESIAN_POINT ( 'NONE',  ( -52.77438362643999881, 65.17411849586700612, -147.9984795835769944 ) ) ;
#5330 = FACE_OUTER_BOUND ( 'NONE', #5118, .T. ) ;
#5331 = LINE ( 'NONE', #7590, #10208 ) ;
#5332 = CARTESIAN_POINT ( 'NONE',  ( -84.73238362644100619, 100.3530677455522238, -147.9984795835769944 ) ) ;
#5333 = CARTESIAN_POINT ( 'NONE',  ( -72.71333998487527595, 97.90337055318686055, -93.68950548826974511 ) ) ;
#5334 = CARTESIAN_POINT ( 'NONE',  ( -52.77438362644100067, 101.5320169952374414, -147.9984795835769944 ) ) ;
#5335 = EDGE_LOOP ( 'NONE', ( #5672, #1669, #3764, #363 ) ) ;
#5336 = CARTESIAN_POINT ( 'NONE',  ( 41.34657265215283672, 39.69837247939362612, 110.6302339309636409 ) ) ;
#5337 = ORIENTED_EDGE ( 'NONE', *, *, #14260, .F. ) ;
#5338 = COLOUR_RGB ( '', 0.66274510, 0.83137255, 0.94901961) ;
#5339 = LINE ( 'NONE', #1758, #4079 ) ;
#5340 = CARTESIAN_POINT ( 'NONE',  ( -1.750120246539717428, -2.256875000000012843, 3.272202384321438284 ) ) ;
#5341 = VERTEX_POINT ( 'NONE', #8159 ) ;
#5342 = VECTOR ( 'NONE', #13369, 1000.000000000000114 ) ;
#5343 = ADVANCED_FACE ( 'NONE', ( #12890 ), #8045, .F. ) ;
#5344 = DIRECTION ( 'NONE',  ( 0.000000000000000000, -0.000000000000000000, -1.000000000000000000 ) ) ;
#5346 = EDGE_CURVE ( 'NONE', #3973, #9206, #5894, .T. ) ;
#5345 = PRODUCT ( 'Mounting Plate', 'Mounting Plate', '', ( #7033 ) ) ;
#5347 = CARTESIAN_POINT ( 'NONE',  ( -13.41835358098578723, 11.39999970914576188, -8.183940086454237317 ) ) ;
#5348 = VECTOR ( 'NONE', #111, 1000.000000000000000 ) ;
#5349 = CLOSED_SHELL ( 'NONE', ( #4045, #6235, #8484, #12288, #14557, #9697, #5563, #2712, #12860, #5869, #12148, #11906, #7809, #12832, #10835 ) ) ;
#5350 = CARTESIAN_POINT ( 'NONE',  ( 3.897114317029974018, 9.945166405816858860E-15, -2.250000000000001332 ) ) ;
#5351 = AXIS2_PLACEMENT_3D ( 'NONE', #14808, #3181, #694 ) ;
#5352 = CARTESIAN_POINT ( 'NONE',  ( -96.77438362643999881, 110.1741184958670061, -79.59847958357700293 ) ) ;
#5353 = DIRECTION ( 'NONE',  ( 0.8660254037844482555, 0.000000000000000000, 0.4999999999999831801 ) ) ;
#5354 = TOROIDAL_SURFACE ( 'NONE', #4105, 3.299999999999474909, 0.2000000000005234813 ) ;
#5355 = DIRECTION ( 'NONE',  ( 0.9961946980917452121, -3.779777825264104572E-17, 0.08715574274766174634 ) ) ;
#5356 = DIRECTION ( 'NONE',  ( 1.000000000000000000, 0.000000000000000000, 0.000000000000000000 ) ) ;
#5357 = EDGE_LOOP ( 'NONE', ( #10352, #11096 ) ) ;
#5358 = CYLINDRICAL_SURFACE ( 'NONE', #5310, 3.000000000000002665 ) ;
#5359 = ORIENTED_EDGE ( 'NONE', *, *, #7103, .T. ) ;
#5360 = ORIENTED_EDGE ( 'NONE', *, *, #11805, .T. ) ;
#5361 = VERTEX_POINT ( 'NONE', #4744 ) ;
#5362 = AXIS2_PLACEMENT_3D ( 'NONE', #8927, #4272, #2805 ) ;
#5363 = ORIENTED_EDGE ( 'NONE', *, *, #6678, .T. ) ;
#5364 = ADVANCED_FACE ( 'NONE', ( #11576 ), #4676, .F. ) ;
#5365 = ORIENTED_EDGE ( 'NONE', *, *, #1242, .T. ) ;
#5366 = AXIS2_PLACEMENT_3D ( 'NONE', #14223, #3605, #7257 ) ;
#5367 = CARTESIAN_POINT ( 'NONE',  ( 3.525223957706937306, -5.967963562373009623, 0.6998565464874195730 ) ) ;
#5368 = VECTOR ( 'NONE', #8813, 1000.000000000000114 ) ;
#5369 = CARTESIAN_POINT ( 'NONE',  ( 0.7224497989600745518, -2.366250000000003517, 3.625028471221638071 ) ) ;
#5370 = EDGE_CURVE ( 'NONE', #11654, #6682, #11807, .T. ) ;
#5371 = EDGE_CURVE ( 'NONE', #14946, #10174, #8795, .T. ) ;
#5372 =( NAMED_UNIT ( * ) SI_UNIT ( $, .STERADIAN. ) SOLID_ANGLE_UNIT ( ) );
#5373 = CARTESIAN_POINT ( 'NONE',  ( 0.7565055315742956754, -3.781249999999899636, 3.808421443275634921 ) ) ;
#5374 = CARTESIAN_POINT ( 'NONE',  ( -77.82438362644001018, 82.17411849586700612, -80.44847958357698303 ) ) ;
#5375 = DIRECTION ( 'NONE',  ( -1.000000000000000000, 0.000000000000000000, 0.000000000000000000 ) ) ;
#5376 = CARTESIAN_POINT ( 'NONE',  ( -4.362044368365340929, -1.127570259384924611E-14, 0.000000000000000000 ) ) ;
#5377 = CARTESIAN_POINT ( 'NONE',  ( -4.296274425956841725, -0.5002988223950231017, 0.02453012155904704325 ) ) ;
#5378 = CIRCLE ( 'NONE', #10556, 11.49999999999999645 ) ;
#5379 = DIRECTION ( 'NONE',  ( 0.8660254037844383745, -0.5000000000000003331, 0.000000000000000000 ) ) ;
#5380 = DIRECTION ( 'NONE',  ( 1.000000000000000000, 0.000000000000000000, 0.000000000000000000 ) ) ;
#5381 = DIRECTION ( 'NONE',  ( 0.000000000000000000, -1.000000000000000000, 0.000000000000000000 ) ) ;
#5382 = CIRCLE ( 'NONE', #14771, 3.749999999999996447 ) ;
#5383 = EDGE_CURVE ( 'NONE', #1528, #1551, #13557, .T. ) ;
#5384 = ORIENTED_EDGE ( 'NONE', *, *, #13550, .T. ) ;
#5385 = AXIS2_PLACEMENT_3D ( 'NONE', #7862, #12596, #4146 ) ;
#5386 = CARTESIAN_POINT ( 'NONE',  ( -50.02438362644000591, 65.17411849586700612, -86.49847958357699440 ) ) ;
#5387 = EDGE_LOOP ( 'NONE', ( #2045, #8049, #5907, #4623 ) ) ;
#5388 = ORIENTED_EDGE ( 'NONE', *, *, #894, .F. ) ;
#5389 = EDGE_LOOP ( 'NONE', ( #7156, #4078, #8139, #9611 ) ) ;
#5390 = ADVANCED_FACE ( 'NONE', ( #5697 ), #10631, .T. ) ;
#5391 = CARTESIAN_POINT ( 'NONE',  ( 14.25000000000000000, -0.2038245569916330158, 23.22168783648699986 ) ) ;
#5392 = VECTOR ( 'NONE', #11756, 1000.000000000000000 ) ;
#5393 = CARTESIAN_POINT ( 'NONE',  ( -3.336666538900096679, -5.084999999999988418, 0.001247370357366475637 ) ) ;
#5394 = EDGE_CURVE ( 'NONE', #9704, #682, #8317, .T. ) ;
#5395 = AXIS2_PLACEMENT_3D ( 'NONE', #8376, #10778, #11706 ) ;
#5396 = EDGE_CURVE ( 'NONE', #13723, #11747, #10304, .T. ) ;
#5397 = DIRECTION ( 'NONE',  ( 0.000000000000000000, -1.000000000000000000, 0.000000000000000000 ) ) ;
#5398 = CARTESIAN_POINT ( 'NONE',  ( -46.58670980944423690, 5.000000000000000000, 91.50956111919106206 ) ) ;
#5399 = DIRECTION ( 'NONE',  ( 0.000000000000000000, 0.000000000000000000, 1.000000000000000000 ) ) ;
#5400 = CARTESIAN_POINT ( 'NONE',  ( -59.02799568714584666, 0.000000000000000000, -73.34256232478206528 ) ) ;
#5401 = CARTESIAN_POINT ( 'NONE',  ( -64.53565528768383786, 67.29799558322736175, -81.84847958357697451 ) ) ;
#5402 = CARTESIAN_POINT ( 'NONE',  ( 1.454275362300765373, -5.407858183789424622, 2.950057805584367809 ) ) ;
#5403 = ORIENTED_EDGE ( 'NONE', *, *, #1095, .T. ) ;
#5404 = AXIS2_PLACEMENT_3D ( 'NONE', #8470, #11034, #245 ) ;
#5405 = DIRECTION ( 'NONE',  ( 0.000000000000000000, -1.000000000000000000, 0.000000000000000000 ) ) ;
#5406 = ORIENTED_EDGE ( 'NONE', *, *, #10238, .T. ) ;
#5407 = VECTOR ( 'NONE', #3875, 1000.000000000000000 ) ;
#5408 = ORIENTED_EDGE ( 'NONE', *, *, #11386, .F. ) ;
#5409 = CARTESIAN_POINT ( 'NONE',  ( -1.859859099471618649, -3.328125000000058620, -3.476502332403788476 ) ) ;
#5410 = ORIENTED_EDGE ( 'NONE', *, *, #3453, .T. ) ;
#5411 = CARTESIAN_POINT ( 'NONE',  ( -9.503456061879928640, -12.00000029085427222, 69.60114695342350899 ) ) ;
#5412 = LINE ( 'NONE', #14845, #2366 ) ;
#5413 = VECTOR ( 'NONE', #788, 1000.000000000000114 ) ;
#5414 = CARTESIAN_POINT ( 'NONE',  ( -16.75000000000000000, -2.500000000000000000, 21.77831216351300014 ) ) ;
#5415 = FACE_OUTER_BOUND ( 'NONE', #6696, .T. ) ;
#5416 = CARTESIAN_POINT ( 'NONE',  ( 2.192040893916867184, 1.873195365144028290, 4.500000000000000888 ) ) ;
#5417 = CARTESIAN_POINT ( 'NONE',  ( -3.031088913245534755, 0.04639863247562457660, 3.749999999999999556 ) ) ;
#5418 = CARTESIAN_POINT ( 'NONE',  ( -69.48563225166269319, 98.17410195967158870, -94.70794860920351255 ) ) ;
#5419 = DIRECTION ( 'NONE',  ( 0.000000000000000000, 1.000000000000000000, 0.000000000000000000 ) ) ;
#5420 = ORIENTED_EDGE ( 'NONE', *, *, #8308, .T. ) ;
#5421 = CIRCLE ( 'NONE', #7888, 2.042000000000002036 ) ;
#5422 = DIRECTION ( 'NONE',  ( 0.000000000000000000, 0.000000000000000000, -1.000000000000000000 ) ) ;
#5423 = CARTESIAN_POINT ( 'NONE',  ( -1.834300037444539955, -0.9131249999999379030, -3.428720741157346819 ) ) ;
#5424 = ORIENTED_EDGE ( 'NONE', *, *, #8833, .F. ) ;
#5425 = CARTESIAN_POINT ( 'NONE',  ( 2.598076211353310239, 1.678847577293378857, -4.499999999999999112 ) ) ;
#5426 = MANIFOLD_SOLID_BREP ( 'Cut-Extrude1[4]', #5349 ) ;
#5427 = CYLINDRICAL_SURFACE ( 'NONE', #14300, 2.000000000000001776 ) ;
#5428 = DIRECTION ( 'NONE',  ( 0.000000000000000000, 0.000000000000000000, 1.000000000000000000 ) ) ;
#5429 = AXIS2_PLACEMENT_3D ( 'NONE', #11461, #10434, #8041 ) ;
#5430 = PLANE ( 'NONE',  #948 ) ;
#5431 = CARTESIAN_POINT ( 'NONE',  ( -15.50000000000000000, -0.1999999999999999556, -22.50000000000000000 ) ) ;
#5432 = EDGE_CURVE ( 'NONE', #3491, #13082, #10519, .T. ) ;
#5433 = CARTESIAN_POINT ( 'NONE',  ( -50.73238362644099197, 97.99516924618178848, -147.9984795835769944 ) ) ;
#5434 = B_SPLINE_CURVE_WITH_KNOTS ( 'NONE', 3,
 ( #7796, #7937, #1967, #14983 ),
 .UNSPECIFIED., .F., .F.,
 ( 4, 4 ),
 ( 0.7672515605989058685, 0.7674537633733152786 ),
 .UNSPECIFIED. ) ;
#5435 = ORIENTED_EDGE ( 'NONE', *, *, #1656, .T. ) ;
#5436 = DIRECTION ( 'NONE',  ( 1.904272108403300901E-17, -1.000000000000000000, -6.513401669715868659E-16 ) ) ;
#5437 = ADVANCED_FACE ( 'NONE', ( #7232 ), #7395, .T. ) ;
#5438 = ORIENTED_EDGE ( 'NONE', *, *, #6779, .T. ) ;
#5439 = ORIENTED_EDGE ( 'NONE', *, *, #2031, .F. ) ;
#5440 = ORIENTED_EDGE ( 'NONE', *, *, #13775, .F. ) ;
#5441 = EDGE_LOOP ( 'NONE', ( #4565, #13424, #10751, #918 ) ) ;
#5442 = EDGE_LOOP ( 'NONE', ( #10273, #7971, #9666, #281 ) ) ;
#5443 = CARTESIAN_POINT ( 'NONE',  ( -3.640430666773472268, -5.483588562373210351, -0.3595019156637501712 ) ) ;
#5444 = CARTESIAN_POINT ( 'NONE',  ( -3.516205069202310352, -0.1631249999999115075, 1.881096664271727059 ) ) ;
#5445 = PLANE ( 'NONE',  #13022 ) ;
#5446 = CARTESIAN_POINT ( 'NONE',  ( 1.584545095770156564, -1.812499999999970912, 3.828300384078624941 ) ) ;
#5447 = DIRECTION ( 'NONE',  ( -0.000000000000000000, 1.000000000000000000, -0.000000000000000000 ) ) ;
#5448 = CARTESIAN_POINT ( 'NONE',  ( 16.75000000000000000, -0.2038245569916320166, -23.22168783648699986 ) ) ;
#5449 = DIRECTION ( 'NONE',  ( -0.000000000000000000, 0.000000000000000000, 1.000000000000000000 ) ) ;
#5450 = CARTESIAN_POINT ( 'NONE',  ( -1.590481721991226172, -1.687500000000021760, 3.843696589995393875 ) ) ;
#5451 = DIRECTION ( 'NONE',  ( -0.000000000000000000, -0.000000000000000000, 1.000000000000000000 ) ) ;
#5452 = EDGE_CURVE ( 'NONE', #704, #11895, #3729, .T. ) ;
#5453 = DIRECTION ( 'NONE',  ( 0.000000000000000000, -1.000000000000000000, 0.000000000000000000 ) ) ;
#5454 = ORIENTED_EDGE ( 'NONE', *, *, #11256, .T. ) ;
#5455 = CARTESIAN_POINT ( 'NONE',  ( -86.27438362644001302, 82.17411849586700612, -152.4984795835769944 ) ) ;
#5456 = EDGE_CURVE ( 'NONE', #5220, #9369, #11307, .T. ) ;
#5457 = ORIENTED_EDGE ( 'NONE', *, *, #14630, .T. ) ;
#5458 = ORIENTED_EDGE ( 'NONE', *, *, #5960, .T. ) ;
#5459 = ORIENTED_EDGE ( 'NONE', *, *, #2600, .F. ) ;
#5460 = DIRECTION ( 'NONE',  ( 1.000000000000000000, 0.000000000000000000, 0.000000000000000000 ) ) ;
#5461 = CARTESIAN_POINT ( 'NONE',  ( 3.333123593314366140, -4.616249999999967990, -0.6642911394208504960 ) ) ;
#5462 = ADVANCED_FACE ( 'NONE', ( #1637, #10798 ), #13435, .F. ) ;
#5463 = DIRECTION ( 'NONE',  ( 1.000000000000000000, 9.422394424380278809E-16, 0.000000000000000000 ) ) ;
#5464 = EDGE_CURVE ( 'NONE', #10251, #3023, #12026, .T. ) ;
#5465 = CARTESIAN_POINT ( 'NONE',  ( 2.573385150445058223, -3.618985300545106920, 0.000000000000000000 ) ) ;
#5466 = CARTESIAN_POINT ( 'NONE',  ( -23.24999999999999289, -5.000000000000000000, -27.00000000000000000 ) ) ;
#5467 = DIRECTION ( 'NONE',  ( -1.000000000000000000, 0.000000000000000000, 0.000000000000000000 ) ) ;
#5468 = CARTESIAN_POINT ( 'NONE',  ( 3.264569842716556369, -0.4995676945082427323, 2.204052319888019085 ) ) ;
#5469 = DIRECTION ( 'NONE',  ( 0.000000000000000000, 0.000000000000000000, 1.000000000000000000 ) ) ;
#5470 = EDGE_CURVE ( 'NONE', #10234, #12733, #6170, .T. ) ;
#5471 = CARTESIAN_POINT ( 'NONE',  ( -0.3227798623957894297, -5.319375000000161613, 3.289865787063878333 ) ) ;
#5472 = ORIENTED_EDGE ( 'NONE', *, *, #9965, .T. ) ;
#5473 = DIRECTION ( 'NONE',  ( 1.000000000000000000, 0.000000000000000000, 0.000000000000000000 ) ) ;
#5474 = EDGE_CURVE ( 'NONE', #11913, #6450, #9619, .T. ) ;
#5475 = ORIENTED_EDGE ( 'NONE', *, *, #11979, .F. ) ;
#5476 = ADVANCED_FACE ( 'NONE', ( #8458 ), #2615, .T. ) ;
#5477 = CARTESIAN_POINT ( 'NONE',  ( -16.75000000000000000, -2.500000000000000000, 23.22168783648699986 ) ) ;
#5478 = ITEM_DEFINED_TRANSFORMATION ( 'NONE', 'NONE', #12194,  #285 ) ;
#5479 = ORIENTED_EDGE ( 'NONE', *, *, #8763, .F. ) ;
#5480 = MANIFOLD_SOLID_BREP ( 'NONE', #9271 ) ;
#5481 = CARTESIAN_POINT ( 'NONE',  ( 0.001544386136394801726, -0.7500000000000344169, 4.283781196144704317 ) ) ;
#5482 = ORIENTED_EDGE ( 'NONE', *, *, #10184, .F. ) ;
#5483 = CARTESIAN_POINT ( 'NONE',  ( -3.899807011409266888, -3.514838562372941233, 0.3830646067729001625 ) ) ;
#5484 = CARTESIAN_POINT ( 'NONE',  ( -89.27438362643999881, 65.17411849586700612, -182.2484795835770228 ) ) ;
#5485 = CARTESIAN_POINT ( 'NONE',  ( 22.58164641901421632, -11.40000029085423705, -8.183940086454239093 ) ) ;
#5486 = CYLINDRICAL_SURFACE ( 'NONE', #4050, 1.250000000000001110 ) ;
#5487 = ADVANCED_FACE ( 'NONE', ( #5519 ), #12038, .T. ) ;
#5488 = CARTESIAN_POINT ( 'NONE',  ( -4.522482571421197584, 11.58578614677263197, 70.03692566716178192 ) ) ;
#5489 = DIRECTION ( 'NONE',  ( -0.000000000000000000, -1.000000000000000000, -0.000000000000000000 ) ) ;
#5490 = PLANE ( 'NONE',  #3370 ) ;
#5491 = DIRECTION ( 'NONE',  ( 0.000000000000000000, 0.000000000000000000, -1.000000000000000000 ) ) ;
#5492 = DIRECTION ( 'NONE',  ( 0.000000000000000000, 0.000000000000000000, 1.000000000000000000 ) ) ;
#5493 = AXIS2_PLACEMENT_3D ( 'NONE', #5835, #7718, #11280 ) ;
#5494 = VERTEX_POINT ( 'NONE', #14875 ) ;
#5495 = VECTOR ( 'NONE', #13989, 1000.000000000000000 ) ;
#5496 = CARTESIAN_POINT ( 'NONE',  ( -3.733522804429754594, -2.085000000000140741, 0.001371824453763029108 ) ) ;
#5497 = ORIENTED_EDGE ( 'NONE', *, *, #10659, .F. ) ;
#5498 = CARTESIAN_POINT ( 'NONE',  ( -69.77438362644001302, 82.17411849586700612, -83.44847958357698303 ) ) ;
#5499 = AXIS2_PLACEMENT_3D ( 'NONE', #9406, #14144, #3519 ) ;
#5500 = CARTESIAN_POINT ( 'NONE',  ( -86.77438362643999881, 65.17411849586700612, -149.9984795835770228 ) ) ;
#5501 = CARTESIAN_POINT ( 'NONE',  ( 17.18107410701653137, -3.642811188889856666, 0.1743669014992923205 ) ) ;
#5502 = VECTOR ( 'NONE', #12435, 1000.000000000000000 ) ;
#5503 = LINE ( 'NONE', #10204, #204 ) ;
#5504 = SURFACE_STYLE_FILL_AREA ( #7755 ) ;
#5505 = DIRECTION ( 'NONE',  ( 0.000000000000000000, 0.000000000000000000, 1.000000000000000000 ) ) ;
#5506 = AXIS2_PLACEMENT_3D ( 'NONE', #9508, #10844, #7363 ) ;
#5507 = FACE_OUTER_BOUND ( 'NONE', #4973, .T. ) ;
#5508 = EDGE_LOOP ( 'NONE', ( #14006, #2017, #3489, #15045, #6472, #9118 ) ) ;
#5509 = DIRECTION ( 'NONE',  ( 0.4999999999999827360, 0.000000000000000000, -0.8660254037844485886 ) ) ;
#5510 = ORIENTED_EDGE ( 'NONE', *, *, #3085, .F. ) ;
#5511 = VECTOR ( 'NONE', #6, 1000.000000000000000 ) ;
#5512 = ORIENTED_EDGE ( 'NONE', *, *, #7430, .T. ) ;
#5513 = CARTESIAN_POINT ( 'NONE',  ( -2.103997734759340155, -5.225624999999808118, 2.565685703212198465 ) ) ;
#5514 = VERTEX_POINT ( 'NONE', #2955 ) ;
#5515 = VERTEX_POINT ( 'NONE', #11327 ) ;
#5516 = EDGE_LOOP ( 'NONE', ( #6364, #2717, #671, #6209 ) ) ;
#5517 = CARTESIAN_POINT ( 'NONE',  ( 2.266335642362669045, -6.139838562372765374, -2.760089361353832427 ) ) ;
#5518 = CARTESIAN_POINT ( 'NONE',  ( -2.976231983981160845, -1.194374999999927578, 2.444352914378567387 ) ) ;
#5519 = FACE_OUTER_BOUND ( 'NONE', #10196, .T. ) ;
#5520 = CARTESIAN_POINT ( 'NONE',  ( -2.240749814637992721, -2.656250000000047073, 3.351605112894145311 ) ) ;
#5521 = LINE ( 'NONE', #2957, #2294 ) ;
#5522 = ADVANCED_FACE ( 'NONE', ( #13812 ), #6619, .T. ) ;
#5523 = CARTESIAN_POINT ( 'NONE',  ( 15.50000000000000000, -0.1999999999999999556, -21.05000000000000426 ) ) ;
#5524 = PRESENTATION_LAYER_ASSIGNMENT (  '', '', ( #8488 ) ) ;
#5525 = CARTESIAN_POINT ( 'NONE',  ( -52.77438362644100067, 99.17411849586700612, -147.9984795835769944 ) ) ;
#5526 = CARTESIAN_POINT ( 'NONE',  ( -2.667636957649788698, -1.359375000000169198, -3.248130456407447575 ) ) ;
#5527 = CARTESIAN_POINT ( 'NONE',  ( 14.25000000000000000, -2.500000000000000000, -21.77831216351300014 ) ) ;
#5528 = DIRECTION ( 'NONE',  ( -0.000000000000000000, 1.000000000000000000, -0.000000000000000000 ) ) ;
#5529 = CARTESIAN_POINT ( 'NONE',  ( -54.81638362644000040, 65.17411849586700612, -147.9984795835769944 ) ) ;
#5530 = EDGE_LOOP ( 'NONE', ( #13181, #11933, #12901, #8512 ) ) ;
#5531 = CARTESIAN_POINT ( 'NONE',  ( -13.16982544356192797, 11.99999970914575975, 0.01788390626213397228 ) ) ;
#5532 = CONICAL_SURFACE ( 'NONE', #12209, 1732.050807568789651, 1.047197551196575871 ) ;
#5533 = ORIENTED_EDGE ( 'NONE', *, *, #13334, .T. ) ;
#5534 = ORIENTED_EDGE ( 'NONE', *, *, #4905, .T. ) ;
#5535 = ORIENTED_EDGE ( 'NONE', *, *, #6246, .F. ) ;
#5536 = CONICAL_SURFACE ( 'NONE', #7273, 8.349999999999996092, 0.7853981633974476129 ) ;
#5537 = DIRECTION ( 'NONE',  ( -0.9378889346118977066, 0.3469356515732558988, 0.000000000000000000 ) ) ;
#5538 = PRODUCT_DEFINITION ( 'UNKNOWN', '', #12950, #7924 ) ;
#5539 = EDGE_CURVE ( 'NONE', #14624, #5090, #7770, .T. ) ;
#5540 = DIRECTION ( 'NONE',  ( 0.000000000000000000, 0.000000000000000000, -1.000000000000000000 ) ) ;
#5541 = DIRECTION ( 'NONE',  ( -0.000000000000000000, -0.000000000000000000, 1.000000000000000000 ) ) ;
#5542 = CIRCLE ( 'NONE', #8735, 1.999999999999989564 ) ;
#5543 = ADVANCED_FACE ( 'NONE', ( #12501 ), #5445, .F. ) ;
#5544 = CIRCLE ( 'NONE', #3540, 2.500000000000002220 ) ;
#5545 = CARTESIAN_POINT ( 'NONE',  ( -85.77438362644001302, 82.17411849586700612, -112.9984795835769944 ) ) ;
#5546 = LINE ( 'NONE', #6860, #5413 ) ;
#5547 = CARTESIAN_POINT ( 'NONE',  ( 3.372444421885775423, -0.4995676945082423992, 2.006840812041871924 ) ) ;
#5548 = CARTESIAN_POINT ( 'NONE',  ( -35.58670980944424400, 0.000000000000000000, 99.29549861919106490 ) ) ;
#5549 = CIRCLE ( 'NONE', #4057, 1.250000000000001110 ) ;
#5550 = ORIENTED_EDGE ( 'NONE', *, *, #1356, .T. ) ;
#5551 = DIRECTION ( 'NONE',  ( 0.000000000000000000, 0.000000000000000000, 1.000000000000000000 ) ) ;
#5552 = ORIENTED_EDGE ( 'NONE', *, *, #398, .F. ) ;
#5553 = ADVANCED_FACE ( 'NONE', ( #9072, #7909, #12640, #6460, #14734 ), #2879, .T. ) ;
#5554 = DIRECTION ( 'NONE',  ( 0.000000000000000000, 0.000000000000000000, -1.000000000000000000 ) ) ;
#5555 = ORIENTED_EDGE ( 'NONE', *, *, #11521, .T. ) ;
#5556 = AXIS2_PLACEMENT_3D ( 'NONE', #11467, #14102, #832 ) ;
#5557 = CARTESIAN_POINT ( 'NONE',  ( 3.016622086615760256, -0.8749999999999454880, 3.018230387793254810 ) ) ;
#5558 = ORIENTED_EDGE ( 'NONE', *, *, #7964, .T. ) ;
#5559 = EDGE_CURVE ( 'NONE', #1481, #2078, #6352, .T. ) ;
#5560 = CARTESIAN_POINT ( 'NONE',  ( 4.043765020089121975, -1.967963562373018949, 0.8054683246621723303 ) ) ;
#5561 = AXIS2_PLACEMENT_3D ( 'NONE', #9410, #5882, #4771 ) ;
#5562 = CARTESIAN_POINT ( 'NONE',  ( -15.50000000000000000, -1.037157890325000054, -18.50000000000000000 ) ) ;
#5563 = ADVANCED_FACE ( 'NONE', ( #544 ), #3106, .T. ) ;
#5564 = PLANE ( 'NONE',  #12780 ) ;
#5565 = EDGE_CURVE ( 'NONE', #11245, #8515, #2006, .T. ) ;
#5566 = DIRECTION ( 'NONE',  ( -0.000000000000000000, 1.000000000000000000, -0.000000000000000000 ) ) ;
#5567 = AXIS2_PLACEMENT_3D ( 'NONE', #10857, #5197, #14635 ) ;
#5568 = DIRECTION ( 'NONE',  ( 0.000000000000000000, 0.000000000000000000, 1.000000000000000000 ) ) ;
#5569 = CARTESIAN_POINT ( 'NONE',  ( 17.18164641901421419, 11.39999970914575833, -0.3335879563140091153 ) ) ;
#5570 = CARTESIAN_POINT ( 'NONE',  ( -86.77438362644001302, 65.17411849586700612, -79.59847958357700293 ) ) ;
#5571 = EDGE_CURVE ( 'NONE', #502, #11643, #7624, .T. ) ;
#5572 = ORIENTED_EDGE ( 'NONE', *, *, #1247, .T. ) ;
#5573 = CARTESIAN_POINT ( 'NONE',  ( -66.41143315690761995, 66.60412428008086749, -83.44847958357698303 ) ) ;
#5574 = CARTESIAN_POINT ( 'NONE',  ( 3.084626646876158063, -5.093749999999860556, -2.059924370567768115 ) ) ;
#5575 = ORIENTED_EDGE ( 'NONE', *, *, #5087, .F. ) ;
#5576 = VECTOR ( 'NONE', #14500, 1000.000000000000000 ) ;
#5577 = VECTOR ( 'NONE', #7279, 1000.000000000000000 ) ;
#5578 = EDGE_CURVE ( 'NONE', #4297, #14050, #4195, .T. ) ;
#5579 = CARTESIAN_POINT ( 'NONE',  ( 2.926652851519762955, -1.694375000000067022, -2.400566300852225776 ) ) ;
#5580 = CARTESIAN_POINT ( 'NONE',  ( -86.77438362643999881, 65.17411849586700612, -145.4984795835769944 ) ) ;
#5581 = DIRECTION ( 'NONE',  ( 0.000000000000000000, 0.000000000000000000, -1.000000000000000000 ) ) ;
#5582 = CARTESIAN_POINT ( 'NONE',  ( 14.25000000000000000, -2.500000000000000000, 21.77831216351300014 ) ) ;
#5583 = DIRECTION ( 'NONE',  ( -2.551930889570660354E-15, 1.000000000000000000, 0.000000000000000000 ) ) ;
#5584 = CARTESIAN_POINT ( 'NONE',  ( 3.530157234965975555, -5.226201182446649440, -2.246195850846843811E-13 ) ) ;
#5585 = CARTESIAN_POINT ( 'NONE',  ( 22.58164641901421632, 12.39999970914576188, -9.367156043074160721 ) ) ;
#5586 = CARTESIAN_POINT ( 'NONE',  ( -8.457587148907983021, 1.075975824879282337E-15, 57.64681057632257222 ) ) ;
#5587 = ORIENTED_EDGE ( 'NONE', *, *, #6232, .T. ) ;
#5588 = CIRCLE ( 'NONE', #13999, 0.2000000000000057288 ) ;
#5589 = DIRECTION ( 'NONE',  ( 0.000000000000000000, 0.000000000000000000, 1.000000000000000000 ) ) ;
#5590 = ORIENTED_EDGE ( 'NONE', *, *, #3844, .T. ) ;
#5591 = ORIENTED_EDGE ( 'NONE', *, *, #11212, .T. ) ;
#5592 = CARTESIAN_POINT ( 'NONE',  ( -2.465526969817839031, -3.960000000000052811, -2.463696919997012014 ) ) ;
#5593 = ORIENTED_EDGE ( 'NONE', *, *, #10869, .T. ) ;
#5594 = VERTEX_POINT ( 'NONE', #12577 ) ;
#5595 = ORIENTED_EDGE ( 'NONE', *, *, #10381, .T. ) ;
#5596 = CARTESIAN_POINT ( 'NONE',  ( -1.713569807928926991, -5.671088562373275188, 3.203872873516009800 ) ) ;
#5597 = PRESENTATION_LAYER_ASSIGNMENT (  '', '', ( #3103 ) ) ;
#5598 = CARTESIAN_POINT ( 'NONE',  ( 3.639928100339127948, -0.5225000000000105116, 1.508827519571796172 ) ) ;
#5599 = VECTOR ( 'NONE', #7979, 1000.000000000000114 ) ;
#5600 = CARTESIAN_POINT ( 'NONE',  ( -56.85838362643999488, 65.17411849586700612, -147.9984795835769944 ) ) ;
#5601 = CIRCLE ( 'NONE', #2862, 0.2000000000005226763 ) ;
#5602 = CARTESIAN_POINT ( 'NONE',  ( 1.567576417386008947, -2.187499999999996447, -3.781634774997608250 ) ) ;
#5603 = CARTESIAN_POINT ( 'NONE',  ( -31.00000000000000000, -2.500000000000000000, 0.000000000000000000 ) ) ;
#5604 = DIRECTION ( 'NONE',  ( -0.000000000000000000, 1.000000000000000000, 0.000000000000000000 ) ) ;
#5605 = CARTESIAN_POINT ( 'NONE',  ( -69.77438362644001302, 71.67411849586700612, -80.44847958357698303 ) ) ;
#5606 = CARTESIAN_POINT ( 'NONE',  ( -1.221455774822097329, -1.296874999999898082, -4.030457444822014956 ) ) ;
#5607 = DIRECTION ( 'NONE',  ( 0.8660254037844387076, 0.4999999999999998890, 0.000000000000000000 ) ) ;
#5608 = CARTESIAN_POINT ( 'NONE',  ( -96.77438362643999881, 104.6741184958670061, -15.85886927678779834 ) ) ;
#5609 = DIRECTION ( 'NONE',  ( -1.000000000000000000, 0.000000000000000000, 0.000000000000000000 ) ) ;
#5610 = MANIFOLD_SOLID_BREP ( '\X2\00d8\X0\4.0mm Dowel Hole1', #5323 ) ;
#5611 = ORIENTED_EDGE ( 'NONE', *, *, #2723, .T. ) ;
#5612 = DIRECTION ( 'NONE',  ( 0.000000000000000000, 0.000000000000000000, -1.000000000000000000 ) ) ;
#5613 = AXIS2_PLACEMENT_3D ( 'NONE', #10806, #4837, #5939 ) ;
#5614 = ORIENTED_EDGE ( 'NONE', *, *, #2432, .F. ) ;
#5615 = CIRCLE ( 'NONE', #13037, 0.2000000000000057288 ) ;
#5616 = ORIENTED_EDGE ( 'NONE', *, *, #436, .T. ) ;
#5617 = ORIENTED_EDGE ( 'NONE', *, *, #2505, .T. ) ;
#5618 = AXIS2_PLACEMENT_3D ( 'NONE', #5183, #2691, #7437 ) ;
#5619 = ADVANCED_FACE ( 'NONE', ( #14954 ), #8806, .T. ) ;
#5620 = CARTESIAN_POINT ( 'NONE',  ( -86.77438362644100778, 101.5320169952374414, -150.4984795835770228 ) ) ;
#5621 = CARTESIAN_POINT ( 'NONE',  ( 2.514916625122327165, 4.927357795815638042, 3.529993346153717244E-16 ) ) ;
#5622 = AXIS2_PLACEMENT_3D ( 'NONE', #6434, #11143, #5251 ) ;
#5623 = CARTESIAN_POINT ( 'NONE',  ( -69.77438362644001302, 82.17411849586700612, -112.9984795835769944 ) ) ;
#5624 = CARTESIAN_POINT ( 'NONE',  ( -14.25000000000000000, -0.2038245569916330158, 21.77831216351300014 ) ) ;
#5625 = CARTESIAN_POINT ( 'NONE',  ( 17.18164641901421419, -3.654316742536411589, 0.2664120436859910845 ) ) ;
#5626 = AXIS2_PLACEMENT_3D ( 'NONE', #6008, #8320, #11960 ) ;
#5627 = DIRECTION ( 'NONE',  ( -1.000000000000000000, 0.000000000000000000, 0.000000000000000000 ) ) ;
#5628 = FACE_OUTER_BOUND ( 'NONE', #8189, .T. ) ;
#5629 = AXIS2_PLACEMENT_3D ( 'NONE', #14448, #4999, #2821 ) ;
#5630 = DIRECTION ( 'NONE',  ( 1.000000000000000000, -0.000000000000000000, 0.000000000000000000 ) ) ;
#5631 = ORIENTED_EDGE ( 'NONE', *, *, #620, .T. ) ;
#5632 = LINE ( 'NONE', #14066, #10323 ) ;
#5633 = EDGE_CURVE ( 'NONE', #8453, #5837, #12081, .T. ) ;
#5634 = EDGE_LOOP ( 'NONE', ( #4902, #14368, #5459, #13616 ) ) ;
#5635 = ORIENTED_EDGE ( 'NONE', *, *, #997, .T. ) ;
#5636 = DIRECTION ( 'NONE',  ( 0.000000000000000000, 0.000000000000000000, -1.000000000000000000 ) ) ;
#5637 = AXIS2_PLACEMENT_3D ( 'NONE', #14685, #11129, #5473 ) ;
#5638 = ORIENTED_EDGE ( 'NONE', *, *, #339, .F. ) ;
#5639 = EDGE_CURVE ( 'NONE', #8947, #5361, #4102, .T. ) ;
#5640 = AXIS2_PLACEMENT_3D ( 'NONE', #4810, #12955, #217 ) ;
#5641 = CARTESIAN_POINT ( 'NONE',  ( -4.238263498634291082, -0.4687499999999378830, -0.8414564874906409475 ) ) ;
#5642 = ORIENTED_EDGE ( 'NONE', *, *, #5394, .F. ) ;
#5643 = CARTESIAN_POINT ( 'NONE',  ( 0.7964824889291316490, -2.217963562373153952, -4.011792787020751483 ) ) ;
#5644 = DIRECTION ( 'NONE',  ( 0.000000000000000000, 1.000000000000000000, 0.000000000000000000 ) ) ;
#5645 = FACE_OUTER_BOUND ( 'NONE', #5530, .T. ) ;
#5646 = AXIS2_PLACEMENT_3D ( 'NONE', #7243, #11968, #14516 ) ;
#5647 = AXIS2_PLACEMENT_3D ( 'NONE', #5267, #9050, #7751 ) ;
#5648 = DIRECTION ( 'NONE',  ( 0.000000000000000000, 1.000000000000000000, 0.000000000000000000 ) ) ;
#5649 = CARTESIAN_POINT ( 'NONE',  ( -70.34862606286944242, 98.16638921377227689, -94.68195642959773295 ) ) ;
#5650 = EDGE_CURVE ( 'NONE', #1386, #11935, #11413, .T. ) ;
#5651 = CARTESIAN_POINT ( 'NONE',  ( -60.52799568714584666, 103.6741184958669919, -73.34256232478206528 ) ) ;
#5652 = PRODUCT_CONTEXT ( 'NONE', #9108, 'mechanical' ) ;
#5653 = ORIENTED_EDGE ( 'NONE', *, *, #13122, .F. ) ;
#5654 = EDGE_CURVE ( 'NONE', #7059, #2214, #9502, .T. ) ;
#5655 = CARTESIAN_POINT ( 'NONE',  ( -3.232499647488480399, -5.421874999999926281, -1.728882681842687452 ) ) ;
#5656 = VERTEX_POINT ( 'NONE', #7353 ) ;
#5657 = VECTOR ( 'NONE', #4749, 1000.000000000000114 ) ;
#5658 = CARTESIAN_POINT ( 'NONE',  ( -1.054465238365572599, -2.881875000000049702, -3.471494129216005753 ) ) ;
#5659 = LINE ( 'NONE', #7821, #1010 ) ;
#5660 = EDGE_CURVE ( 'NONE', #12429, #13931, #11037, .T. ) ;
#5661 = FACE_OUTER_BOUND ( 'NONE', #12200, .T. ) ;
#5662 = CARTESIAN_POINT ( 'NONE',  ( -61.64938362644000591, 82.17411849586700612, -93.49847958357699440 ) ) ;
#5663 = FACE_BOUND ( 'NONE', #10648, .T. ) ;
#5664 = CYLINDRICAL_SURFACE ( 'NONE', #7259, 1.785937500000001066 ) ;
#5665 = CARTESIAN_POINT ( 'NONE',  ( -91.02438362644100778, 99.17411849586700612, -149.9984795835770228 ) ) ;
#5666 = EDGE_CURVE ( 'NONE', #13685, #5306, #13878, .T. ) ;
#5667 = APPLICATION_CONTEXT ( 'automotive_design' ) ;
#5668 = FACE_OUTER_BOUND ( 'NONE', #6510, .T. ) ;
#5669 = CONICAL_SURFACE ( 'NONE', #13588, 7.999999999992790656, 0.7853981634258691003 ) ;
#5670 = ORIENTED_EDGE ( 'NONE', *, *, #10272, .F. ) ;
#5671 = DIRECTION ( 'NONE',  ( 1.000000000000000000, 0.000000000000000000, 0.000000000000000000 ) ) ;
#5672 = ORIENTED_EDGE ( 'NONE', *, *, #5673, .T. ) ;
#5673 = EDGE_CURVE ( 'NONE', #14751, #382, #10533, .T. ) ;
#5674 = ORIENTED_EDGE ( 'NONE', *, *, #11826, .F. ) ;
#5675 = EDGE_CURVE ( 'NONE', #12970, #12826, #14980, .T. ) ;
#5676 = CARTESIAN_POINT ( 'NONE',  ( -0.3313405146687902203, -4.850625000000119869, -3.351331461923205080 ) ) ;
#5677 = ORIENTED_EDGE ( 'NONE', *, *, #514, .F. ) ;
#5678 = ORIENTED_EDGE ( 'NONE', *, *, #10965, .F. ) ;
#5679 = EDGE_LOOP ( 'NONE', ( #6192, #5025 ) ) ;
#5680 = LINE ( 'NONE', #4418, #3579 ) ;
#5681 = CARTESIAN_POINT ( 'NONE',  ( -3.978984329191358693, -0.08500000000000000611, -3.334211887901014441E-13 ) ) ;
#5682 = AXIS2_PLACEMENT_3D ( 'NONE', #5973, #8127, #4640 ) ;
#5683 = CARTESIAN_POINT ( 'NONE',  ( -15.50000000000000000, 0.000000000000000000, -26.50000000000000000 ) ) ;
#5684 = CARTESIAN_POINT ( 'NONE',  ( 3.935506471057187206, -2.046874999999910738, -1.192685225358429912 ) ) ;
#5685 = CARTESIAN_POINT ( 'NONE',  ( -82.52438362643998460, 65.17411849586700612, -145.4984795835769944 ) ) ;
#5686 = PLANE ( 'NONE',  #4145 ) ;
#5687 = CARTESIAN_POINT ( 'NONE',  ( -4.296275033669348709, -0.4995676945082693776, 0.008185550287844470252 ) ) ;
#5688 = CARTESIAN_POINT ( 'NONE',  ( -69.77438362644001302, 82.17411849586700612, -150.4984795835769944 ) ) ;
#5689 = CARTESIAN_POINT ( 'NONE',  ( -69.77438362644001302, 82.17411849586700612, -79.59847958357700293 ) ) ;
#5690 = ORIENTED_EDGE ( 'NONE', *, *, #15106, .F. ) ;
#5691 = CARTESIAN_POINT ( 'NONE',  ( -15.50000000000000000, -0.2038245569916614930, -23.94337567297399971 ) ) ;
#5692 = ORIENTED_EDGE ( 'NONE', *, *, #8316, .F. ) ;
#5693 = ORIENTED_EDGE ( 'NONE', *, *, #967, .T. ) ;
#5694 = ORIENTED_EDGE ( 'NONE', *, *, #3761, .F. ) ;
#5695 = DIRECTION ( 'NONE',  ( 0.000000000000000000, 0.000000000000000000, -1.000000000000000000 ) ) ;
#5696 = CARTESIAN_POINT ( 'NONE',  ( 1.592243150387700146, -4.756875000000070131, -2.981552405995577359 ) ) ;
#5697 = FACE_OUTER_BOUND ( 'NONE', #5872, .T. ) ;
#5698 = LINE ( 'NONE', #6708, #11444 ) ;
#5699 = DIRECTION ( 'NONE',  ( 2.551930889570660354E-15, -1.000000000000000000, 0.000000000000000000 ) ) ;
#5700 = DIRECTION ( 'NONE',  ( 0.000000000000000000, 1.000000000000000000, 0.000000000000000000 ) ) ;
#5701 = CARTESIAN_POINT ( 'NONE',  ( -9.797174393178927223E-17, 9.500000000000000000, 0.000000000000000000 ) ) ;
#5702 = CARTESIAN_POINT ( 'NONE',  ( 22.58164641901421632, -12.00000029085423670, -11.73358795631401463 ) ) ;
#5703 = CYLINDRICAL_SURFACE ( 'NONE', #4829, 4.000000000000000888 ) ;
#5704 = EDGE_LOOP ( 'NONE', ( #7722, #2620, #2431, #12174 ) ) ;
#5705 = DIRECTION ( 'NONE',  ( 0.000000000000000000, 0.000000000000000000, 1.000000000000000000 ) ) ;
#5706 = ORIENTED_EDGE ( 'NONE', *, *, #10178, .T. ) ;
#5707 = EDGE_LOOP ( 'NONE', ( #15093, #14119 ) ) ;
#5708 = CARTESIAN_POINT ( 'NONE',  ( -79.02077156573416516, 103.6741184958669777, -73.34256232478206528 ) ) ;
#5709 = ORIENTED_EDGE ( 'NONE', *, *, #7727, .F. ) ;
#5710 = CARTESIAN_POINT ( 'NONE',  ( -1.612261674935887568, -1.312500000000171863, -3.888369303904286589 ) ) ;
#5711 = ORIENTED_EDGE ( 'NONE', *, *, #11382, .T. ) ;
#5712 = CARTESIAN_POINT ( 'NONE',  ( 2.899850257105391904, -2.124213562373065134, -2.901953948755849222 ) ) ;
#5713 = DIRECTION ( 'NONE',  ( 1.000000000000000000, -0.000000000000000000, 1.224646799147353207E-16 ) ) ;
#5714 = EDGE_CURVE ( 'NONE', #14910, #4229, #1211, .T. ) ;
#5715 = CARTESIAN_POINT ( 'NONE',  ( -68.41221392010733382, 90.17411849586700612, -58.99847958357691624 ) ) ;
#5716 = DIRECTION ( 'NONE',  ( 0.000000000000000000, 0.000000000000000000, 1.000000000000000000 ) ) ;
#5717 = EDGE_CURVE ( 'NONE', #1201, #13826, #3624, .T. ) ;
#5718 = CYLINDRICAL_SURFACE ( 'NONE', #11992, 0.6000000000000000888 ) ;
#5719 = ORIENTED_EDGE ( 'NONE', *, *, #11321, .T. ) ;
#5720 = CYLINDRICAL_SURFACE ( 'NONE', #6143, 2.500000000000002220 ) ;
#5721 = CARTESIAN_POINT ( 'NONE',  ( -86.77438362644100778, 99.17411849586700612, -145.4984795835769944 ) ) ;
#5722 = VERTEX_POINT ( 'NONE', #5683 ) ;
#5723 = DIRECTION ( 'NONE',  ( 0.000000000000000000, 0.000000000000000000, 1.000000000000000000 ) ) ;
#5724 = CARTESIAN_POINT ( 'NONE',  ( -0.7178551545708362625, -5.281249999999999112, -3.613793911565672534 ) ) ;
#5725 = ORIENTED_EDGE ( 'NONE', *, *, #7721, .F. ) ;
#5726 = EDGE_CURVE ( 'NONE', #6907, #6162, #14246, .T. ) ;
#5727 = CARTESIAN_POINT ( 'NONE',  ( -1.418005212499557466, -2.272500000000021281, 3.426931839692804349 ) ) ;
#5728 = EDGE_CURVE ( 'NONE', #5594, #13232, #8312, .T. ) ;
#5729 = DIRECTION ( 'NONE',  ( 0.000000000000000000, 0.000000000000000000, 1.000000000000000000 ) ) ;
#5730 = DIRECTION ( 'NONE',  ( -1.000000000000000000, -1.747085166004344019E-15, 0.000000000000000000 ) ) ;
#5731 = CARTESIAN_POINT ( 'NONE',  ( 3.826752640285553397, -0.4995676945082493381, 1.002635565222667280 ) ) ;
#5732 = DIRECTION ( 'NONE',  ( 0.000000000000000000, 0.000000000000000000, 1.000000000000000000 ) ) ;
#5733 = CARTESIAN_POINT ( 'NONE',  ( -69.77438362644001302, 82.17411849586700612, -3.496191900462991775 ) ) ;
#5734 = CIRCLE ( 'NONE', #3994, 1.500000000000001332 ) ;
#5735 = ORIENTED_EDGE ( 'NONE', *, *, #9039, .F. ) ;
#5736 = CARTESIAN_POINT ( 'NONE',  ( -14.25000000000000000, -2.500000000000000000, 21.77831216351300014 ) ) ;
#5737 = VERTEX_POINT ( 'NONE', #6355 ) ;
#5738 = EDGE_CURVE ( 'NONE', #12429, #858, #8057, .T. ) ;
#5739 = VERTEX_POINT ( 'NONE', #10987 ) ;
#5740 = CARTESIAN_POINT ( 'NONE',  ( 3.151910583997930004, -4.522499999999531894, 1.304188709559742643 ) ) ;
#5741 = ORIENTED_EDGE ( 'NONE', *, *, #197, .T. ) ;
#5742 = EDGE_CURVE ( 'NONE', #449, #9860, #14544, .T. ) ;
#5743 = ORIENTED_EDGE ( 'NONE', *, *, #15200, .T. ) ;
#5744 = EDGE_LOOP ( 'NONE', ( #1031, #7136, #10256, #1088 ) ) ;
#5745 = CIRCLE ( 'NONE', #14871, 4.249999999999996447 ) ;
#5746 = CARTESIAN_POINT ( 'NONE',  ( 3.654558516219509556, -4.967963562373524766, 0.7279234453325641452 ) ) ;
#5747 = CARTESIAN_POINT ( 'NONE',  ( -3.865847815970003154, -1.085000000000063469, -0.001011349278461548453 ) ) ;
#5748 = EDGE_CURVE ( 'NONE', #11599, #1408, #13559, .T. ) ;
#5749 = AXIS2_PLACEMENT_3D ( 'NONE', #10813, #178, #5867 ) ;
#5750 = CARTESIAN_POINT ( 'NONE',  ( -2.876356209513419415, -2.375000000000007994, -2.877876508394843658 ) ) ;
#5751 = PLANE ( 'NONE',  #9225 ) ;
#5752 = CARTESIAN_POINT ( 'NONE',  ( -96.77438362643999881, 65.17411849586700612, -15.85886927678779834 ) ) ;
#5753 = EDGE_CURVE ( 'NONE', #8984, #12668, #5244, .T. ) ;
#5754 = EDGE_CURVE ( 'NONE', #897, #1574, #439, .T. ) ;
#5755 = CARTESIAN_POINT ( 'NONE',  ( -15.50000000000000000, -0.2000000000000000111, 22.50000000000000000 ) ) ;
#5756 = CARTESIAN_POINT ( 'NONE',  ( 15.50000000000000000, -2.500000000000000000, 23.94337567297399971 ) ) ;
#5757 = DIRECTION ( 'NONE',  ( 1.000000000000000000, -0.000000000000000000, -0.000000000000000000 ) ) ;
#5758 = CARTESIAN_POINT ( 'NONE',  ( -4.522482571421201136, -12.00000029085427222, 70.03692566716181034 ) ) ;
#5759 = ORIENTED_EDGE ( 'NONE', *, *, #12940, .T. ) ;
#5760 = FACE_OUTER_BOUND ( 'NONE', #12056, .T. ) ;
#5761 = ORIENTED_EDGE ( 'NONE', *, *, #6419, .F. ) ;
#5762 = ADVANCED_FACE ( 'NONE', ( #9814 ), #9962, .F. ) ;
#5763 = VERTEX_POINT ( 'NONE', #13325 ) ;
#5764 = ORIENTED_EDGE ( 'NONE', *, *, #10649, .F. ) ;
#5765 = CARTESIAN_POINT ( 'NONE',  ( -89.52438362644001302, 65.17411849586700612, -145.4984795835769660 ) ) ;
#5766 = CARTESIAN_POINT ( 'NONE',  ( 3.384491019838401726, -4.600625000000129639, -0.3324735777645301260 ) ) ;
#5767 = EDGE_CURVE ( 'NONE', #14049, #8186, #2754, .T. ) ;
#5768 = CIRCLE ( 'NONE', #782, 0.2500000000000000000 ) ;
#5769 = CARTESIAN_POINT ( 'NONE',  ( -88.81638362644100937, 100.3530677455522238, -147.9984795835769944 ) ) ;
#5770 = CARTESIAN_POINT ( 'NONE',  ( -67.13357088347154900, 75.17411849586700612, -44.45439862457403990 ) ) ;
#5771 = CARTESIAN_POINT ( 'NONE',  ( -1.120937138223994101, 2.242130364943868859, -4.499999999999998224 ) ) ;
#5772 = FACE_OUTER_BOUND ( 'NONE', #8910, .T. ) ;
#5773 = AXIS2_PLACEMENT_3D ( 'NONE', #365, #13636, #6584 ) ;
#5774 = CARTESIAN_POINT ( 'NONE',  ( -90.85838362644101096, 99.17411849586700612, -147.9984795835769944 ) ) ;
#5775 = DIRECTION ( 'NONE',  ( 1.000000000000000000, 0.000000000000000000, 0.000000000000000000 ) ) ;
#5776 = DIRECTION ( 'NONE',  ( 0.000000000000000000, 1.000000000000000000, 0.000000000000000000 ) ) ;
#5777 = AXIS2_PLACEMENT_3D ( 'NONE', #4443, #5699, #9162 ) ;
#5778 = CARTESIAN_POINT ( 'NONE',  ( -50.73238362644099197, 99.17411849586700612, -147.9984795835769944 ) ) ;
#5779 = EDGE_LOOP ( 'NONE', ( #5285, #13278, #7012, #14158 ) ) ;
#5780 = CARTESIAN_POINT ( 'NONE',  ( -69.77438362644001302, 82.17411849586700612, -67.69567958357700377 ) ) ;
#5781 = ORIENTED_EDGE ( 'NONE', *, *, #7230, .T. ) ;
#5782 = ORIENTED_EDGE ( 'NONE', *, *, #12108, .T. ) ;
#5783 = ORIENTED_EDGE ( 'NONE', *, *, #4227, .F. ) ;
#5784 = CARTESIAN_POINT ( 'NONE',  ( 1.584545095770156564, -1.812499999999970912, 3.828300384078624941 ) ) ;
#5785 = VERTEX_POINT ( 'NONE', #14694 ) ;
#5786 = VECTOR ( 'NONE', #6462, 1000.000000000000000 ) ;
#5787 = CARTESIAN_POINT ( 'NONE',  ( 3.675079574260619708, -3.061713562373090003, -1.523835802059044564 ) ) ;
#5788 = DIRECTION ( 'NONE',  ( 0.000000000000000000, 0.000000000000000000, 1.000000000000000000 ) ) ;
#5789 = DIRECTION ( 'NONE',  ( 0.000000000000000000, 0.000000000000000000, -1.000000000000000000 ) ) ;
#5790 = VECTOR ( 'NONE', #14475, 1000.000000000000000 ) ;
#5791 = CARTESIAN_POINT ( 'NONE',  ( -60.52799568714584666, 60.67411849586701322, -73.34256232478206528 ) ) ;
#5792 = FACE_OUTER_BOUND ( 'NONE', #795, .T. ) ;
#5793 = ORIENTED_EDGE ( 'NONE', *, *, #10067, .T. ) ;
#5794 = DIRECTION ( 'NONE',  ( -0.8660254037844387076, -0.4999999999999998890, 0.000000000000000000 ) ) ;
#5795 = CIRCLE ( 'NONE', #6303, 2.042000000000002036 ) ;
#5796 = TOROIDAL_SURFACE ( 'NONE', #14447, 1.200000000000000178, 0.6000000000000000888 ) ;
#5797 = DIRECTION ( 'NONE',  ( 0.000000000000000000, 1.000000000000000000, 0.000000000000000000 ) ) ;
#5798 = CARTESIAN_POINT ( 'NONE',  ( 13.47019165201499646, -11.81169222820027365, -63.19206102791760316 ) ) ;
#5799 = ORIENTED_EDGE ( 'NONE', *, *, #7043, .F. ) ;
#5800 = CIRCLE ( 'NONE', #9006, 4.500000000000003553 ) ;
#5801 =( NAMED_UNIT ( * ) SI_UNIT ( $, .STERADIAN. ) SOLID_ANGLE_UNIT ( ) );
#5802 = CARTESIAN_POINT ( 'NONE',  ( 1.415591119045080504, -5.187499999999808153, -3.415035020420910783 ) ) ;
#5803 = ORIENTED_EDGE ( 'NONE', *, *, #4605, .F. ) ;
#5804 = EDGE_CURVE ( 'NONE', #4340, #9489, #336, .T. ) ;
#5805 = CARTESIAN_POINT ( 'NONE',  ( -3.717546150574369879, -2.069374999999891607, -0.3671215460811757536 ) ) ;
#5806 = AXIS2_PLACEMENT_3D ( 'NONE', #8164, #9467, #1019 ) ;
#5807 = CARTESIAN_POINT ( 'NONE',  ( 40.52020888806953991, -24.00000000000000000, 6.000000000000000000 ) ) ;
#5808 = CIRCLE ( 'NONE', #5059, 4.499999999999997335 ) ;
#5809 = DIRECTION ( 'NONE',  ( -0.000000000000000000, 1.000000000000000000, -0.000000000000000000 ) ) ;
#5810 = DIRECTION ( 'NONE',  ( 0.000000000000000000, 0.000000000000000000, 1.000000000000000000 ) ) ;
#5811 = CARTESIAN_POINT ( 'NONE',  ( 22.58164641901421632, 11.99999970914576330, -11.73358795631400397 ) ) ;
#5812 = DIRECTION ( 'NONE',  ( 0.000000000000000000, 0.000000000000000000, 1.000000000000000000 ) ) ;
#5813 = DIRECTION ( 'NONE',  ( 0.000000000000000000, -1.000000000000000000, 0.000000000000000000 ) ) ;
#5814 = VERTEX_POINT ( 'NONE', #10041 ) ;
#5815 = CARTESIAN_POINT ( 'NONE',  ( -86.77438362643999881, 65.17411849586700612, -182.2484795835770228 ) ) ;
#5816 = CIRCLE ( 'NONE', #5072, 1.785937500000001066 ) ;
#5817 = CIRCLE ( 'NONE', #592, 4.499999999999997335 ) ;
#5818 = ADVANCED_FACE ( 'NONE', ( #7586 ), #14776, .T. ) ;
#5819 = VECTOR ( 'NONE', #9982, 1000.000000000000000 ) ;
#5820 = ORIENTED_EDGE ( 'NONE', *, *, #7251, .T. ) ;
#5821 = ORIENTED_EDGE ( 'NONE', *, *, #982, .T. ) ;
#5822 = VERTEX_POINT ( 'NONE', #12224 ) ;
#5823 = VERTEX_POINT ( 'NONE', #1602 ) ;
#5824 = EDGE_CURVE ( 'NONE', #4974, #4158, #3105, .T. ) ;
#5825 = VERTEX_POINT ( 'NONE', #6494 ) ;
#5826 = CARTESIAN_POINT ( 'NONE',  ( 1.807163061527332415, -4.171088562373018505, -3.378841529629734719 ) ) ;
#5827 = DIRECTION ( 'NONE',  ( -1.000000000000000000, 0.000000000000000000, 0.000000000000000000 ) ) ;
#5828 = DIRECTION ( 'NONE',  ( 0.000000000000000000, 0.000000000000000000, -1.000000000000000000 ) ) ;
#5829 = DIRECTION ( 'NONE',  ( 1.000000000000000000, 0.000000000000000000, 0.000000000000000000 ) ) ;
#5830 = AXIS2_PLACEMENT_3D ( 'NONE', #8005, #11503, #4373 ) ;
#5831 = DIRECTION ( 'NONE',  ( 0.000000000000000000, 1.000000000000000000, 0.000000000000000000 ) ) ;
#5832 = LINE ( 'NONE', #3793, #10346 ) ;
#5833 = CARTESIAN_POINT ( 'NONE',  ( -55.47438362644099641, 99.17411849586700612, -145.2984795835770058 ) ) ;
#5834 = CARTESIAN_POINT ( 'NONE',  ( 17.14647606710965988, 3.654220075139516855, 0.2671853888517377595 ) ) ;
#5835 = CARTESIAN_POINT ( 'NONE',  ( -12.81835358098578403, 11.99999970914576330, -11.73358795631400753 ) ) ;
#5836 = LINE ( 'NONE', #5758, #6786 ) ;
#5837 = VERTEX_POINT ( 'NONE', #1518 ) ;
#5838 = CARTESIAN_POINT ( 'NONE',  ( 1.403561989263862998E-14, -5.500000000000001776, 0.000000000000000000 ) ) ;
#5839 = EDGE_CURVE ( 'NONE', #4923, #3175, #11771, .T. ) ;
#5840 = ORIENTED_EDGE ( 'NONE', *, *, #13237, .T. ) ;
#5841 = ORIENTED_EDGE ( 'NONE', *, *, #14053, .F. ) ;
#5842 = ORIENTED_EDGE ( 'NONE', *, *, #8100, .T. ) ;
#5843 = COLOUR_RGB ( '', 0.09019608, 0.27058824, 0.51372549) ;
#5844 = EDGE_CURVE ( 'NONE', #6768, #14868, #1680, .T. ) ;
#5845 = VECTOR ( 'NONE', #2685, 1000.000000000000114 ) ;
#5846 = FACE_OUTER_BOUND ( 'NONE', #7922, .T. ) ;
#5847 = ADVANCED_FACE ( 'NONE', ( #6428 ), #5328, .F. ) ;
#5848 = CIRCLE ( 'NONE', #3598, 8.124999999999992895 ) ;
#5849 = CARTESIAN_POINT ( 'NONE',  ( -3.581969766213484174, -3.100624999999847198, 0.3518610084922548231 ) ) ;
#5850 = DIRECTION ( 'NONE',  ( -1.000000000000000000, 0.000000000000000000, 0.000000000000000000 ) ) ;
#5851 = CARTESIAN_POINT ( 'NONE',  ( 22.58164641901421632, -3.579317323512964499, -0.3335879563140091153 ) ) ;
#5852 = CARTESIAN_POINT ( 'NONE',  ( -52.77438362644100067, 101.5320169952374414, -147.9984795835769944 ) ) ;
#5853 = DIRECTION ( 'NONE',  ( 0.000000000000000000, 0.000000000000000000, 1.000000000000000000 ) ) ;
#5854 = EDGE_CURVE ( 'NONE', #7225, #11930, #12548, .T. ) ;
#5855 = CARTESIAN_POINT ( 'NONE',  ( 16.75000000000000000, -2.500000000000000000, -21.77831216351300014 ) ) ;
#5856 = CARTESIAN_POINT ( 'NONE',  ( -52.77438362643999881, 65.17411849586700612, -150.4984795835770228 ) ) ;
#5857 = AXIS2_PLACEMENT_3D ( 'NONE', #4319, #15005, #11530 ) ;
#5858 = DIRECTION ( 'NONE',  ( -0.003614861529252313879, -4.336780354824422708E-16, 0.9999934663667180423 ) ) ;
#5859 = CARTESIAN_POINT ( 'NONE',  ( -66.41143315690761995, 66.60412428008086749, -83.44847958357698303 ) ) ;
#5860 = CIRCLE ( 'NONE', #2127, 4.499999999999997335 ) ;
#5861 = EDGE_LOOP ( 'NONE', ( #3021, #2305, #1260, #1490, #12769 ) ) ;
#5862 = VECTOR ( 'NONE', #7220, 1000.000000000000000 ) ;
#5863 = LINE ( 'NONE', #9168, #7625 ) ;
#5864 = EDGE_CURVE ( 'NONE', #4158, #15328, #14471, .T. ) ;
#5865 = ORIENTED_EDGE ( 'NONE', *, *, #13775, .T. ) ;
#5866 = VERTEX_POINT ( 'NONE', #5102 ) ;
#5867 = DIRECTION ( 'NONE',  ( 0.000000000000000000, 0.000000000000000000, 1.000000000000000000 ) ) ;
#5868 = ORIENTED_EDGE ( 'NONE', *, *, #14059, .T. ) ;
#5869 = ADVANCED_FACE ( 'NONE', ( #12613 ), #9259, .F. ) ;
#5870 = DIRECTION ( 'NONE',  ( 0.000000000000000000, 0.000000000000000000, -1.000000000000000000 ) ) ;
#5871 = ADVANCED_FACE ( 'NONE', ( #1974 ), #5564, .F. ) ;
#5872 = EDGE_LOOP ( 'NONE', ( #10853, #14363, #12097, #1126, #13301 ) ) ;
#5873 = AXIS2_PLACEMENT_3D ( 'NONE', #14589, #702, #9930 ) ;
#5874 = B_SPLINE_CURVE_WITH_KNOTS ( 'NONE', 3,
 ( #13495, #5040, #8904, #13645, #6374, #11088, #6222, #2861, #10930, #14489, #8605, #1542, #6297, #14714, #7608, #4103, #12331, #6446, #11157, #3950, #13418, #3877, #2708, #8830, #13575, #7452, #12698, #9125, #6740, #2070, #6820, #7896, #5731, #977, #6597, #13863 ),
 .UNSPECIFIED., .F., .F.,
 ( 4, 2, 2, 2, 2, 2, 2, 2, 2, 2, 2, 2, 2, 2, 2, 2, 2, 4 ),
 ( 0.000000000000000000, 0.0009396455755520615426, 0.001879291151104123085, 0.002818936726656184628, 0.003758582302208246170, 0.004698227877760306412, 0.005637873453312367521, 0.006577519028864427762, 0.007517164604416488871, 0.008456810179968549113, 0.009396455755520611089, 0.01033610133107267307, 0.01127574690662473504, 0.01221539248217679355, 0.01315503805772885379, 0.01362486084550488565, 0.01409468363328091750, 0.01503432920883297774 ),
 .UNSPECIFIED. ) ;
#5875 = CARTESIAN_POINT ( 'NONE',  ( -3.751644922634416179, -2.436713562373012731, -1.555143193707982929 ) ) ;
#5876 = CONICAL_SURFACE ( 'NONE', #4118, 1732.050807568785558, 1.047197551196574761 ) ;
#5877 = AXIS2_PLACEMENT_3D ( 'NONE', #10895, #11190, #2737 ) ;
#5878 = LINE ( 'NONE', #8178, #9693 ) ;
#5879 = LINE ( 'NONE', #10580, #6121 ) ;
#5880 = DIRECTION ( 'NONE',  ( 0.000000000000000000, 0.000000000000000000, -1.000000000000000000 ) ) ;
#5881 = PRODUCT_DEFINITION_SHAPE ( 'NONE', 'NONE',  #15342 ) ;
#5882 = DIRECTION ( 'NONE',  ( 1.000000000000000000, -0.000000000000000000, 0.000000000000000000 ) ) ;
#5883 = ORIENTED_EDGE ( 'NONE', *, *, #1810, .T. ) ;
#5884 = AXIS2_PLACEMENT_3D ( 'NONE', #7777, #12510, #1717 ) ;
#5885 = DIRECTION ( 'NONE',  ( 0.000000000000000000, 0.000000000000000000, 1.000000000000000000 ) ) ;
#5886 = DIRECTION ( 'NONE',  ( 0.000000000000000000, 1.000000000000000000, 0.000000000000000000 ) ) ;
#5887 = VECTOR ( 'NONE', #2033, 1000.000000000000000 ) ;
#5888 = EDGE_LOOP ( 'NONE', ( #2681, #15065, #6016, #12637, #5337, #12217, #13357, #12112, #4972, #952, #11410 ) ) ;
#5889 = CARTESIAN_POINT ( 'NONE',  ( -82.27438362643999881, 99.17411849586700612, -86.49847958357699440 ) ) ;
#5890 = CARTESIAN_POINT ( 'NONE',  ( 1.148200974759843618, -0.3818749999999526135, 3.788695824010691382 ) ) ;
#5891 = VERTEX_POINT ( 'NONE', #961 ) ;
#5892 = VECTOR ( 'NONE', #6344, 1000.000000000000000 ) ;
#5893 = CARTESIAN_POINT ( 'NONE',  ( 1.412068586280907923, -2.397499999999971099, 3.411535633775557574 ) ) ;
#5894 = B_SPLINE_CURVE_WITH_KNOTS ( 'NONE', 3,
 ( #6927, #2338, #12818, #13133, #7003, #12976 ),
 .UNSPECIFIED., .F., .F.,
 ( 4, 2, 4 ),
 ( 0.0002380763768130567115, 0.7291065797294590256, 1.457975083082104995 ),
 .UNSPECIFIED. ) ;
#5895 = DIRECTION ( 'NONE',  ( 0.000000000000000000, 0.000000000000000000, -1.000000000000000000 ) ) ;
#5896 = CIRCLE ( 'NONE', #2652, 8.050000000000000711 ) ;
#5897 = DIRECTION ( 'NONE',  ( 0.000000000000000000, 0.000000000000000000, 1.000000000000000000 ) ) ;
#5898 = CARTESIAN_POINT ( 'NONE',  ( 0.8000000000000117018, 9.015594676761164550, 9.797174393178967899E-17 ) ) ;
#5899 = DIRECTION ( 'NONE',  ( -1.000000000000000000, -0.000000000000000000, -0.000000000000000000 ) ) ;
#5900 = FACE_BOUND ( 'NONE', #6018, .T. ) ;
#5901 = DIRECTION ( 'NONE',  ( -1.000000000000000000, 0.000000000000000000, 0.000000000000000000 ) ) ;
#5902 = DIRECTION ( 'NONE',  ( -0.000000000000000000, -0.000000000000000000, 1.000000000000000000 ) ) ;
#5903 = ORIENTED_EDGE ( 'NONE', *, *, #4124, .F. ) ;
#5904 = CARTESIAN_POINT ( 'NONE',  ( -77.89938362643999881, 82.17411849586700612, -150.4984795835769944 ) ) ;
#5905 = ORIENTED_EDGE ( 'NONE', *, *, #3200, .F. ) ;
#5906 = VECTOR ( 'NONE', #7716, 1000.000000000000000 ) ;
#5907 = ORIENTED_EDGE ( 'NONE', *, *, #9240, .F. ) ;
#5908 = ORIENTED_EDGE ( 'NONE', *, *, #2407, .T. ) ;
#5909 = ORIENTED_EDGE ( 'NONE', *, *, #8292, .F. ) ;
#5910 = ORIENTED_EDGE ( 'NONE', *, *, #11407, .T. ) ;
#5911 = CARTESIAN_POINT ( 'NONE',  ( 1.464250807817800482, -4.186713562373068243, -3.538677689569500906 ) ) ;
#5912 = DIRECTION ( 'NONE',  ( 1.000000000000000000, 0.000000000000000000, 0.000000000000000000 ) ) ;
#5913 = CARTESIAN_POINT ( 'NONE',  ( -30.00000000000000000, -5.000000000000000000, -43.00000000000002132 ) ) ;
#5914 = CARTESIAN_POINT ( 'NONE',  ( -16.75000000000000000, -2.500000000000000000, -21.77831216351300014 ) ) ;
#5915 = ADVANCED_FACE ( 'NONE', ( #2130 ), #14514, .F. ) ;
#5916 = CYLINDRICAL_SURFACE ( 'NONE', #3141, 5.500000000000005329 ) ;
#5917 = DIRECTION ( 'NONE',  ( -0.000000000000000000, -0.000000000000000000, 1.000000000000000000 ) ) ;
#5918 = DIRECTION ( 'NONE',  ( 0.000000000000000000, 0.000000000000000000, -1.000000000000000000 ) ) ;
#5919 = DIRECTION ( 'NONE',  ( 0.000000000000000000, 0.000000000000000000, 1.000000000000000000 ) ) ;
#5920 = EDGE_CURVE ( 'NONE', #10374, #9201, #10247, .T. ) ;
#5921 = CARTESIAN_POINT ( 'NONE',  ( -0.3421672931279376995, -3.850625000000083009, -3.483230393025887661 ) ) ;
#5922 = DIRECTION ( 'NONE',  ( 1.000000000000000000, 0.000000000000000000, 0.000000000000000000 ) ) ;
#5923 = ORIENTED_EDGE ( 'NONE', *, *, #8207, .T. ) ;
#5924 = CARTESIAN_POINT ( 'NONE',  ( -69.77438362644001302, 94.57411849586699759, -93.49847958357699440 ) ) ;
#5925 = EDGE_LOOP ( 'NONE', ( #12131, #8519, #3450, #7618 ) ) ;
#5926 = VERTEX_POINT ( 'NONE', #4535 ) ;
#5927 = ORIENTED_EDGE ( 'NONE', *, *, #6624, .T. ) ;
#5928 = AXIS2_PLACEMENT_3D ( 'NONE', #5755, #4574, #7913 ) ;
#5929 = FACE_OUTER_BOUND ( 'NONE', #8639, .T. ) ;
#5930 = CARTESIAN_POINT ( 'NONE',  ( 2.315514200798038047, -2.725624999999891607, -2.819975302942780537 ) ) ;
#5931 = DIRECTION ( 'NONE',  ( 0.000000000000000000, 0.000000000000000000, -1.000000000000000000 ) ) ;
#5932 = LINE ( 'NONE', #77, #3514 ) ;
#5933 = CYLINDRICAL_SURFACE ( 'NONE', #15151, 3.000000000000002665 ) ;
#5934 = ADVANCED_FACE ( 'NONE', ( #6801 ), #4386, .F. ) ;
#5935 = CARTESIAN_POINT ( 'NONE',  ( -15.50000000000000000, 0.000000000000000000, -22.50000000000000000 ) ) ;
#5936 = CARTESIAN_POINT ( 'NONE',  ( -35.58670980944424400, 0.000000000000000000, 95.72362361919107343 ) ) ;
#5937 = CARTESIAN_POINT ( 'NONE',  ( 1.634139617129772404, -12.00000029085424025, -0.3335879563140197179 ) ) ;
#5938 = CYLINDRICAL_SURFACE ( 'NONE', #9785, 8.124999999999992895 ) ;
#5939 = DIRECTION ( 'NONE',  ( 0.000000000000000000, 0.000000000000000000, 1.000000000000000000 ) ) ;
#5940 = ADVANCED_FACE ( 'NONE', ( #9107 ), #13295, .T. ) ;
#5941 = DIRECTION ( 'NONE',  ( -0.000000000000000000, 4.336808689942017736E-16, -1.000000000000000000 ) ) ;
#5942 = VECTOR ( 'NONE', #3628, 1000.000000000000114 ) ;
#5943 = ORIENTED_EDGE ( 'NONE', *, *, #2772, .T. ) ;
#5944 = CARTESIAN_POINT ( 'NONE',  ( -69.77438362644001302, 81.46011849586699327, -83.44847958357698303 ) ) ;
#5945 = ORIENTED_EDGE ( 'NONE', *, *, #8476, .T. ) ;
#5946 = ORIENTED_EDGE ( 'NONE', *, *, #5958, .F. ) ;
#5947 = CARTESIAN_POINT ( 'NONE',  ( -69.77438362644100778, 92.17411849586700612, -67.49847958357700861 ) ) ;
#5948 = EDGE_CURVE ( 'NONE', #9306, #13359, #4614, .T. ) ;
#5949 = CARTESIAN_POINT ( 'NONE',  ( 1.278996873743735163, 0.2031250000000478229, 4.220359392353129735 ) ) ;
#5950 = VERTEX_POINT ( 'NONE', #883 ) ;
#5951 = EDGE_CURVE ( 'NONE', #2123, #3176, #14261, .T. ) ;
#5952 = CARTESIAN_POINT ( 'NONE',  ( -4.294764374624453040, -0.5148395451705815029, 0.4218660116795628356 ) ) ;
#5953 = AXIS2_PLACEMENT_3D ( 'NONE', #2758, #14549, #4002 ) ;
#5954 = LINE ( 'NONE', #1347, #9192 ) ;
#5955 = EDGE_CURVE ( 'NONE', #9472, #16, #14016, .T. ) ;
#5956 = CARTESIAN_POINT ( 'NONE',  ( -64.53565528768383786, 67.29799558322736175, -81.84847958357697451 ) ) ;
#5957 = DIRECTION ( 'NONE',  ( -0.000000000000000000, 0.000000000000000000, -1.000000000000000000 ) ) ;
#5958 = EDGE_CURVE ( 'NONE', #9229, #9845, #13920, .T. ) ;
#5959 = CARTESIAN_POINT ( 'NONE',  ( -50.73238362644099197, 100.3530677455522238, -150.4984795835770228 ) ) ;
#5960 = EDGE_CURVE ( 'NONE', #12176, #14022, #5412, .T. ) ;
#5961 = VERTEX_POINT ( 'NONE', #5485 ) ;
#5962 = CARTESIAN_POINT ( 'NONE',  ( 15.50000000000000000, -5.000000000000000000, -22.50000000000000000 ) ) ;
#5963 = CARTESIAN_POINT ( 'NONE',  ( 14.25000000000000000, -2.500000000000000000, 23.22168783648699986 ) ) ;
#5964 = APPLICATION_PROTOCOL_DEFINITION ( 'draft international standard', 'automotive_design', 1998, #289 ) ;
#5965 = ORIENTED_EDGE ( 'NONE', *, *, #8577, .F. ) ;
#5966 = CARTESIAN_POINT ( 'NONE',  ( -3.160451915950723389, -4.406249999999939604, -2.110071460981538749 ) ) ;
#5967 = ORIENTED_EDGE ( 'NONE', *, *, #12401, .F. ) ;
#5968 = DIRECTION ( 'NONE',  ( -0.4999999999999998890, 0.8660254037844387076, 0.000000000000000000 ) ) ;
#5969 = ADVANCED_FACE ( 'NONE', ( #5645 ), #10185, .F. ) ;
#5970 = CARTESIAN_POINT ( 'NONE',  ( -16.75000000000000000, -2.500000000000000000, 21.77831216351300014 ) ) ;
#5971 = CARTESIAN_POINT ( 'NONE',  ( -84.73238362643999722, 66.35306774555222376, -147.9984795835769944 ) ) ;
#5972 = DIRECTION ( 'NONE',  ( -1.000000000000000000, 0.000000000000000000, 0.000000000000000000 ) ) ;
#5973 = CARTESIAN_POINT ( 'NONE',  ( -90.85838362644101096, 99.17411849586700612, -147.9984795835769944 ) ) ;
#5974 = LINE ( 'NONE', #3629, #4040 ) ;
#5975 = CARTESIAN_POINT ( 'NONE',  ( -73.80978675135780520, 64.78624853950366003, -81.84847958357697451 ) ) ;
#5976 = CYLINDRICAL_SURFACE ( 'NONE', #2522, 17.00000000000000000 ) ;
#5977 = ORIENTED_EDGE ( 'NONE', *, *, #5383, .T. ) ;
#5978 = DIRECTION ( 'NONE',  ( -1.000000000000000000, 0.000000000000000000, 0.000000000000000000 ) ) ;
#5979 = ORIENTED_EDGE ( 'NONE', *, *, #4149, .T. ) ;
#5980 = CYLINDRICAL_SURFACE ( 'NONE', #13497, 0.5999999999999998668 ) ;
#5981 = CARTESIAN_POINT ( 'NONE',  ( -2.795825449145424191, -2.975624999999864517, -2.292747793747711427 ) ) ;
#5982 = ORIENTED_EDGE ( 'NONE', *, *, #3917, .F. ) ;
#5983 = EDGE_LOOP ( 'NONE', ( #2232, #13467, #5204 ) ) ;
#5984 = VERTEX_POINT ( 'NONE', #3291 ) ;
#5985 = CARTESIAN_POINT ( 'NONE',  ( -0.3733708913937817675, -4.264838562373088671, -3.801067638221671263 ) ) ;
#5986 = CARTESIAN_POINT ( 'NONE',  ( -69.77438362644001302, 81.46011849586699327, -83.44847958357698303 ) ) ;
#5987 = CARTESIAN_POINT ( 'NONE',  ( -3.897114317029974462, -9.945166405816860437E-15, 2.249999999999999112 ) ) ;
#5988 = LINE ( 'NONE', #7667, #6770 ) ;
#5989 = DIRECTION ( 'NONE',  ( -0.8660254037844387076, -0.4999999999999998890, 0.000000000000000000 ) ) ;
#5990 = B_SPLINE_CURVE_WITH_KNOTS ( 'NONE', 3,
 ( #6716, #10252, #12377, #4223, #6417, #2912 ),
 .UNSPECIFIED., .F., .F.,
 ( 4, 2, 4 ),
 ( 0.0002380763768115301549, 0.7291065797294569162, 1.457975083082102330 ),
 .UNSPECIFIED. ) ;
#5991 = PLANE ( 'NONE',  #6181 ) ;
#5992 = CYLINDRICAL_SURFACE ( 'NONE', #4256, 2.750000000000002665 ) ;
#5993 = DIRECTION ( 'NONE',  ( -0.4999999999999832356, 0.000000000000000000, -0.8660254037844483666 ) ) ;
#5994 = CARTESIAN_POINT ( 'NONE',  ( 2.255458548909140770, -3.444374999999939568, 2.746210667320699184 ) ) ;
#5995 = DIRECTION ( 'NONE',  ( 0.000000000000000000, 0.000000000000000000, -1.000000000000000000 ) ) ;
#5996 = ORIENTED_EDGE ( 'NONE', *, *, #1992, .T. ) ;
#5997 = DIRECTION ( 'NONE',  ( -1.000000000000000000, 0.000000000000000000, -0.000000000000000000 ) ) ;
#5998 = ORIENTED_EDGE ( 'NONE', *, *, #2198, .T. ) ;
#5999 = CIRCLE ( 'NONE', #11179, 17.00000000000000000 ) ;
#6000 = ORIENTED_EDGE ( 'NONE', *, *, #249, .T. ) ;
#6001 = ORIENTED_EDGE ( 'NONE', *, *, #15071, .F. ) ;
#6002 = DIRECTION ( 'NONE',  ( 1.000000000000000000, -0.000000000000000000, 1.224646799147353207E-16 ) ) ;
#6003 = CARTESIAN_POINT ( 'NONE',  ( 1.974738715674944078, -3.428749999999933795, 2.957050713271639708 ) ) ;
#6004 = ADVANCED_FACE ( 'NONE', ( #13697, #7807 ), #9033, .T. ) ;
#6005 = DIRECTION ( 'NONE',  ( 0.000000000000000000, 0.000000000000000000, 1.000000000000000000 ) ) ;
#6006 = LINE ( 'NONE', #14286, #4763 ) ;
#6007 = FACE_BOUND ( 'NONE', #12987, .T. ) ;
#6008 = CARTESIAN_POINT ( 'NONE',  ( -62.27438362644000591, 74.17411849586699191, -58.99847958357700151 ) ) ;
#6009 = CONICAL_SURFACE ( 'NONE', #7958, 3.968749999999992895, 0.7155849933176756661 ) ;
#6010 = CARTESIAN_POINT ( 'NONE',  ( -96.77438362643999881, 104.6741184958670061, -79.59847958357700293 ) ) ;
#6011 = DIRECTION ( 'NONE',  ( -1.000000000000000000, 0.000000000000000000, 0.000000000000000000 ) ) ;
#6012 = DIRECTION ( 'NONE',  ( 0.000000000000000000, 1.000000000000000000, 0.000000000000000000 ) ) ;
#6013 = CARTESIAN_POINT ( 'NONE',  ( -59.02799568714584666, 103.6741184958669919, -79.59847958357700293 ) ) ;
#6014 = CARTESIAN_POINT ( 'NONE',  ( 23.25000000000000000, -5.000000000000000000, 27.00000000000000000 ) ) ;
#6015 = AXIS2_PLACEMENT_3D ( 'NONE', #10729, #8474, #6183 ) ;
#6016 = ORIENTED_EDGE ( 'NONE', *, *, #8119, .F. ) ;
#6017 = DIRECTION ( 'NONE',  ( -0.08715574274766123286, 0.000000000000000000, 0.9961946980917453232 ) ) ;
#6018 = EDGE_LOOP ( 'NONE', ( #4802, #2307 ) ) ;
#6019 = ORIENTED_EDGE ( 'NONE', *, *, #1662, .T. ) ;
#6020 = ORIENTED_EDGE ( 'NONE', *, *, #10917, .T. ) ;
#6021 = CARTESIAN_POINT ( 'NONE',  ( -57.27438362644000591, 99.17411849586700612, -145.4984795835769660 ) ) ;
#6022 = PRODUCT_RELATED_PRODUCT_CATEGORY ( 'part', '', ( #9435 ) ) ;
#6023 = EDGE_CURVE ( 'NONE', #14332, #14841, #5860, .T. ) ;
#6024 = AXIS2_PLACEMENT_3D ( 'NONE', #7490, #1883, #5162 ) ;
#6025 = CARTESIAN_POINT ( 'NONE',  ( -2.461334822302656100, 0.3437500000001206257, 3.681509895155765655 ) ) ;
#6026 = VERTEX_POINT ( 'NONE', #1266 ) ;
#6027 = CARTESIAN_POINT ( 'NONE',  ( -3.189069343666966372, -6.084999999999998188, 0.000000000000000000 ) ) ;
#6028 = CARTESIAN_POINT ( 'NONE',  ( -52.77438362643999881, 65.17411849586700612, -145.2984795835770058 ) ) ;
#6029 = CIRCLE ( 'NONE', #5268, 1.250000000000001110 ) ;
#6030 = LINE ( 'NONE', #1348, #390 ) ;
#6031 = DIRECTION ( 'NONE',  ( 0.000000000000000000, 0.000000000000000000, 1.000000000000000000 ) ) ;
#6032 = COLOUR_RGB ( '', 0.72549020, 0.75294118, 0.79215686) ;
#6033 = ADVANCED_FACE ( 'NONE', ( #1196 ), #2506, .T. ) ;
#6034 = CARTESIAN_POINT ( 'NONE',  ( -48.27438362644000591, 99.17411849586700612, -79.59847958357700293 ) ) ;
#6035 = ORIENTED_EDGE ( 'NONE', *, *, #3814, .F. ) ;
#6036 = FACE_OUTER_BOUND ( 'NONE', #282, .T. ) ;
#6037 = CARTESIAN_POINT ( 'NONE',  ( 16.95294013567761837, 11.57155134438803223, 0.2884598355027922501 ) ) ;
#6038 = AXIS2_PLACEMENT_3D ( 'NONE', #7397, #9771, #8393 ) ;
#6039 = APPLICATION_PROTOCOL_DEFINITION ( 'draft international standard', 'automotive_design', 1998, #9899 ) ;
#6040 = EDGE_CURVE ( 'NONE', #9472, #2388, #8413, .T. ) ;
#6041 = ORIENTED_EDGE ( 'NONE', *, *, #14470, .T. ) ;
#6042 = CARTESIAN_POINT ( 'NONE',  ( 0.7565055315742956754, -3.781249999999899636, 3.808421443275634921 ) ) ;
#6043 = ORIENTED_EDGE ( 'NONE', *, *, #10348, .T. ) ;
#6044 = EDGE_CURVE ( 'NONE', #13867, #1293, #9796, .T. ) ;
#6045 = VECTOR ( 'NONE', #8166, 1000.000000000000000 ) ;
#6046 = EDGE_CURVE ( 'NONE', #8280, #14101, #5615, .T. ) ;
#6047 = CARTESIAN_POINT ( 'NONE',  ( 3.258191480560199693, -0.6787499999999294653, -2.178773987163739267 ) ) ;
#6048 = DIRECTION ( 'NONE',  ( 1.000000000000000000, -0.000000000000000000, 0.000000000000000000 ) ) ;
#6049 = CIRCLE ( 'NONE', #3063, 2.000000000000001776 ) ;
#6050 = ADVANCED_FACE ( 'NONE', ( #6109 ), #14374, .F. ) ;
#6051 = DIRECTION ( 'NONE',  ( 0.000000000000000000, 1.000000000000000000, 0.000000000000000000 ) ) ;
#6052 = DIRECTION ( 'NONE',  ( -1.000000000000000000, -2.551930889570659960E-15, 0.000000000000000000 ) ) ;
#6053 = AXIS2_PLACEMENT_3D ( 'NONE', #9150, #13665, #5381 ) ;
#6054 = ORIENTED_EDGE ( 'NONE', *, *, #14640, .F. ) ;
#6055 = DIRECTION ( 'NONE',  ( -1.000000000000000000, 0.000000000000000000, 0.000000000000000000 ) ) ;
#6056 = EDGE_CURVE ( 'NONE', #957, #10550, #6030, .T. ) ;
#6057 = ORIENTED_EDGE ( 'NONE', *, *, #12120, .T. ) ;
#6058 = DIRECTION ( 'NONE',  ( 0.000000000000000000, 0.000000000000000000, -1.000000000000000000 ) ) ;
#6059 = CARTESIAN_POINT ( 'NONE',  ( 3.463329978863732173, -3.616249999999970210, -0.6879750677194341746 ) ) ;
#6060 = ORIENTED_EDGE ( 'NONE', *, *, #5675, .T. ) ;
#6061 = ORIENTED_EDGE ( 'NONE', *, *, #912, .T. ) ;
#6062 = AXIS2_PLACEMENT_3D ( 'NONE', #401, #3734, #14509 ) ;
#6063 = CIRCLE ( 'NONE', #7539, 2.699999999999993960 ) ;
#6064 = ORIENTED_EDGE ( 'NONE', *, *, #3814, .T. ) ;
#6065 = PLANE ( 'NONE',  #1836 ) ;
#6066 = AXIS2_PLACEMENT_3D ( 'NONE', #11754, #1200, #8109 ) ;
#6067 = DIRECTION ( 'NONE',  ( 0.000000000000000000, -1.000000000000000000, 0.000000000000000000 ) ) ;
#6068 = FACE_OUTER_BOUND ( 'NONE', #6905, .T. ) ;
#6069 = CARTESIAN_POINT ( 'NONE',  ( -54.81638362644100226, 97.99516924618178848, -147.9984795835769944 ) ) ;
#6070 = FILL_AREA_STYLE_COLOUR ( '', #14423 ) ;
#6071 = FACE_OUTER_BOUND ( 'NONE', #127, .T. ) ;
#6072 = CLOSED_SHELL ( 'NONE', ( #15116, #6960, #2562, #15215, #9629, #10941, #10664, #18 ) ) ;
#6073 = AXIS2_PLACEMENT_3D ( 'NONE', #1389, #11862, #12954 ) ;
#6074 = CIRCLE ( 'NONE', #8026, 4.000000000000004441 ) ;
#6075 = CARTESIAN_POINT ( 'NONE',  ( -1.685726645313963434, -3.256874999999974651, 3.156579729352138486 ) ) ;
#6076 = DIRECTION ( 'NONE',  ( -1.000000000000000000, 0.000000000000000000, 0.000000000000000000 ) ) ;
#6077 = ORIENTED_EDGE ( 'NONE', *, *, #4298, .F. ) ;
#6078 = DIRECTION ( 'NONE',  ( -1.000000000000000000, 0.000000000000000000, 0.000000000000000000 ) ) ;
#6079 = ORIENTED_EDGE ( 'NONE', *, *, #2994, .F. ) ;
#6080 = ORIENTED_EDGE ( 'NONE', *, *, #1858, .T. ) ;
#6081 = ORIENTED_EDGE ( 'NONE', *, *, #11101, .T. ) ;
#6082 = DIRECTION ( 'NONE',  ( -0.9961946980917453232, 7.200509705930738460E-17, -0.08715574274766157981 ) ) ;
#6083 = VECTOR ( 'NONE', #589, 999.9999999999998863 ) ;
#6084 = VECTOR ( 'NONE', #3879, 1000.000000000000000 ) ;
#6085 = CARTESIAN_POINT ( 'NONE',  ( -0.0009180086920793713474, -3.334999999999859632, 3.568205616840286698 ) ) ;
#6086 = CIRCLE ( 'NONE', #14227, 4.500000000000003553 ) ;
#6087 = DIRECTION ( 'NONE',  ( 0.000000000000000000, 0.000000000000000000, 1.000000000000000000 ) ) ;
#6088 = DIRECTION ( 'NONE',  ( 1.287488025362404182E-15, 1.000000000000000000, 0.000000000000000000 ) ) ;
#6089 = CYLINDRICAL_SURFACE ( 'NONE', #13694, 0.8000000000000113687 ) ;
#6090 = LINE ( 'NONE', #81, #11801 ) ;
#6091 = CARTESIAN_POINT ( 'NONE',  ( -16.75000000000000000, -0.2038245569916330158, 23.22168783648699986 ) ) ;
#6092 = CARTESIAN_POINT ( 'NONE',  ( -71.44964421664191434, 89.17411849586702033, -44.18949531478440917 ) ) ;
#6093 = CARTESIAN_POINT ( 'NONE',  ( 15.50000000000000000, -0.4000000000005274892, -22.50000000000000000 ) ) ;
#6094 = PLANE ( 'NONE',  #8323 ) ;
#6095 = CARTESIAN_POINT ( 'NONE',  ( -1.006616814747114065E-29, -2.568816543514387226E-44, 0.000000000000000000 ) ) ;
#6096 = ORIENTED_EDGE ( 'NONE', *, *, #1838, .F. ) ;
#6097 = DIRECTION ( 'NONE',  ( 0.000000000000000000, -1.000000000000000000, -0.000000000000000000 ) ) ;
#6098 = EDGE_CURVE ( 'NONE', #632, #11758, #10820, .T. ) ;
#6099 = ORIENTED_EDGE ( 'NONE', *, *, #6968, .F. ) ;
#6100 = AXIS2_PLACEMENT_3D ( 'NONE', #1322, #1485, #164 ) ;
#6101 = ORIENTED_EDGE ( 'NONE', *, *, #11303, .T. ) ;
#6102 = CIRCLE ( 'NONE', #3107, 1.500000000000001332 ) ;
#6103 = FACE_OUTER_BOUND ( 'NONE', #3221, .T. ) ;
#6104 = DIRECTION ( 'NONE',  ( 1.000000000000000000, 0.000000000000000000, 0.000000000000000000 ) ) ;
#6105 = ORIENTED_EDGE ( 'NONE', *, *, #10376, .T. ) ;
#6106 = CARTESIAN_POINT ( 'NONE',  ( 1.951466014313916641, -1.827338562372905040, 3.653265138806914170 ) ) ;
#6107 = CIRCLE ( 'NONE', #5095, 0.1999999999999987899 ) ;
#6108 = LINE ( 'NONE', #9639, #15137 ) ;
#6109 = FACE_OUTER_BOUND ( 'NONE', #4921, .T. ) ;
#6110 = AXIS2_PLACEMENT_3D ( 'NONE', #3696, #9213, #13953 ) ;
#6111 = PLANE ( 'NONE',  #14696 ) ;
#6112 = VECTOR ( 'NONE', #14408, 1000.000000000000000 ) ;
#6113 = ADVANCED_FACE ( 'NONE', ( #2356 ), #5876, .F. ) ;
#6114 = LINE ( 'NONE', #9876, #7226 ) ;
#6115 = ORIENTED_EDGE ( 'NONE', *, *, #224, .F. ) ;
#6116 = DIRECTION ( 'NONE',  ( -1.000000000000000000, -7.475397945009582610E-16, 0.000000000000000000 ) ) ;
#6117 = ADVANCED_FACE ( 'NONE', ( #10736 ), #4931, .F. ) ;
#6118 = DIRECTION ( 'NONE',  ( 0.000000000000000000, 0.000000000000000000, 1.000000000000000000 ) ) ;
#6119 = VECTOR ( 'NONE', #3669, 1000.000000000000114 ) ;
#6120 = ORIENTED_EDGE ( 'NONE', *, *, #10634, .T. ) ;
#6121 = VECTOR ( 'NONE', #3520, 1000.000000000000114 ) ;
#6122 = SURFACE_SIDE_STYLE ('',( #7269 ) ) ;
#6123 = CARTESIAN_POINT ( 'NONE',  ( 2.712400463490634017, -4.125000000000058620, -2.714386550172725787 ) ) ;
#6124 = ORIENTED_EDGE ( 'NONE', *, *, #3544, .T. ) ;
#6125 = VECTOR ( 'NONE', #9037, 1000.000000000000000 ) ;
#6126 = CARTESIAN_POINT ( 'NONE',  ( 1.112125432426118499, -1.381875000000161391, 3.661359949639011901 ) ) ;
#6127 = CARTESIAN_POINT ( 'NONE',  ( -2.206715255075134774, -5.334838156314726021, 2.588775985198231488 ) ) ;
#6128 = EDGE_CURVE ( 'NONE', #6732, #14103, #1117, .T. ) ;
#6129 = LINE ( 'NONE', #7510, #6815 ) ;
#6130 = AXIS2_PLACEMENT_3D ( 'NONE', #547, #11105, #8775 ) ;
#6131 = CARTESIAN_POINT ( 'NONE',  ( -65.90140028023257912, 89.17411849586700612, -44.99847958359791988 ) ) ;
#6132 = DIRECTION ( 'NONE',  ( 0.000000000000000000, 0.000000000000000000, -1.000000000000000000 ) ) ;
#6133 = COLOUR_RGB ( '', 0.09019608, 0.27058824, 0.51372549) ;
#6134 = CARTESIAN_POINT ( 'NONE',  ( -86.77438362644100778, 101.5320169952374414, -147.9984795835769944 ) ) ;
#6135 = CARTESIAN_POINT ( 'NONE',  ( -69.77438362644001302, 82.17411849586700612, -83.44847958357698303 ) ) ;
#6136 = EDGE_CURVE ( 'NONE', #14050, #4013, #14992, .T. ) ;
#6137 = ORIENTED_EDGE ( 'NONE', *, *, #5571, .F. ) ;
#6138 = DIRECTION ( 'NONE',  ( 0.000000000000000000, 0.000000000000000000, -1.000000000000000000 ) ) ;
#6139 = VERTEX_POINT ( 'NONE', #13085 ) ;
#6140 = FACE_OUTER_BOUND ( 'NONE', #8054, .T. ) ;
#6141 = CARTESIAN_POINT ( 'NONE',  ( 3.039561480324906473, -2.678749999999966214, -2.029833227700064135 ) ) ;
#6142 = EDGE_LOOP ( 'NONE', ( #6365, #1187, #10031, #11778 ) ) ;
#6143 = AXIS2_PLACEMENT_3D ( 'NONE', #7191, #8111, #9412 ) ;
#6144 = EDGE_LOOP ( 'NONE', ( #5555, #6680, #6602, #15295 ) ) ;
#6145 = VERTEX_POINT ( 'NONE', #9563 ) ;
#6146 = CIRCLE ( 'NONE', #6638, 16.06499999999999773 ) ;
#6147 = ADVANCED_FACE ( 'NONE', ( #10497, #9339, #14078, #13154, #11904 ), #9407, .F. ) ;
#6148 = ADVANCED_FACE ( 'NONE', ( #8179, #8343 ), #99, .T. ) ;
#6149 = LINE ( 'NONE', #4961, #8025 ) ;
#6150 = CARTESIAN_POINT ( 'NONE',  ( -3.675091696978340039, 2.375954066961606603, 2.634554458358997042 ) ) ;
#6151 = EDGE_CURVE ( 'NONE', #449, #1588, #4697, .T. ) ;
#6152 = PLANE ( 'NONE',  #5567 ) ;
#6153 = CARTESIAN_POINT ( 'NONE',  ( -1.733190484027876455, 0.04649911033016842360, 4.500000000000000888 ) ) ;
#6154 = FACE_BOUND ( 'NONE', #5357, .T. ) ;
#6155 = AXIS2_PLACEMENT_3D ( 'NONE', #5780, #3508, #11740 ) ;
#6156 = DIRECTION ( 'NONE',  ( 0.5000000000000003331, 0.8660254037844384856, 0.000000000000000000 ) ) ;
#6157 = CARTESIAN_POINT ( 'NONE',  ( -3.069066067673428932, -4.006874999999906706, -1.638984897852511891 ) ) ;
#6158 = EDGE_CURVE ( 'NONE', #9613, #5234, #5879, .T. ) ;
#6159 = CARTESIAN_POINT ( 'NONE',  ( 1.581646419014216542, -12.00000029085424202, 0.2664120436859911956 ) ) ;
#6160 = VECTOR ( 'NONE', #14789, 1000.000000000000000 ) ;
#6161 = EDGE_CURVE ( 'NONE', #12055, #11016, #10049, .T. ) ;
#6162 = VERTEX_POINT ( 'NONE', #5081 ) ;
#6163 = ORIENTED_EDGE ( 'NONE', *, *, #4111, .F. ) ;
#6164 = ORIENTED_EDGE ( 'NONE', *, *, #7082, .F. ) ;
#6165 = VERTEX_POINT ( 'NONE', #13383 ) ;
#6166 = EDGE_LOOP ( 'NONE', ( #2248, #6307, #3002, #13788 ) ) ;
#6167 = FACE_OUTER_BOUND ( 'NONE', #1192, .T. ) ;
#6168 = CARTESIAN_POINT ( 'NONE',  ( 2.743301530724824744, -3.475625000000028386, 2.252549412313605615 ) ) ;
#6169 = AXIS2_PLACEMENT_3D ( 'NONE', #12211, #14899, #12294 ) ;
#6170 = LINE ( 'NONE', #4911, #14732 ) ;
#6171 = CARTESIAN_POINT ( 'NONE',  ( 3.104176526174651229, -4.906250000000120792, 2.075311058921220919 ) ) ;
#6172 = FACE_OUTER_BOUND ( 'NONE', #12363, .T. ) ;
#6173 = DIRECTION ( 'NONE',  ( 0.000000000000000000, 0.000000000000000000, -1.000000000000000000 ) ) ;
#6174 = CYLINDRICAL_SURFACE ( 'NONE', #2166, 4.500000000000003553 ) ;
#6175 = DIRECTION ( 'NONE',  ( 0.000000000000000000, 0.000000000000000000, -1.000000000000000000 ) ) ;
#6176 = DIRECTION ( 'NONE',  ( 0.000000000000000000, 0.000000000000000000, -1.000000000000000000 ) ) ;
#6177 = FACE_OUTER_BOUND ( 'NONE', #6922, .T. ) ;
#6178 = ORIENTED_EDGE ( 'NONE', *, *, #9061, .F. ) ;
#6179 = DIRECTION ( 'NONE',  ( -1.000000000000000000, -2.551930889570659960E-15, 0.000000000000000000 ) ) ;
#6180 = ORIENTED_EDGE ( 'NONE', *, *, #9766, .F. ) ;
#6181 = AXIS2_PLACEMENT_3D ( 'NONE', #8523, #13268, #10538 ) ;
#6182 = ORIENTED_EDGE ( 'NONE', *, *, #4046, .F. ) ;
#6183 = DIRECTION ( 'NONE',  ( -1.000000000000000000, 0.000000000000000000, 0.000000000000000000 ) ) ;
#6184 = CARTESIAN_POINT ( 'NONE',  ( -0.7999999999999912736, -5.500000000000002665, 0.000000000000000000 ) ) ;
#6185 = CARTESIAN_POINT ( 'NONE',  ( -2.972130888462442222, -1.374213562373086450, -2.969983195655016672 ) ) ;
#6186 = PLANE ( 'NONE',  #13055 ) ;
#6187 = FACE_OUTER_BOUND ( 'NONE', #5779, .T. ) ;
#6188 = CARTESIAN_POINT ( 'NONE',  ( -4.296391350416484123, -0.4995676945082700438, -1.627175273956673067E-05 ) ) ;
#6189 = CIRCLE ( 'NONE', #5186, 2.042000000000002036 ) ;
#6190 = FACE_OUTER_BOUND ( 'NONE', #7292, .T. ) ;
#6191 = CARTESIAN_POINT ( 'NONE',  ( -50.27438362643999881, 65.17411849586700612, -79.59847958357700293 ) ) ;
#6192 = ORIENTED_EDGE ( 'NONE', *, *, #12068, .T. ) ;
#6193 = DIRECTION ( 'NONE',  ( 0.000000000000000000, 0.000000000000000000, 1.000000000000000000 ) ) ;
#6194 = APPLICATION_PROTOCOL_DEFINITION ( 'draft international standard', 'automotive_design', 1998, #884 ) ;
#6195 = EDGE_LOOP ( 'NONE', ( #12592, #9745 ) ) ;
#6196 = AXIS2_PLACEMENT_3D ( 'NONE', #964, #12461, #1977 ) ;
#6197 = FILL_AREA_STYLE_COLOUR ( '', #12278 ) ;
#6198 = CARTESIAN_POINT ( 'NONE',  ( -3.269128917323805172, -3.406249999999943601, -2.185603562728522853 ) ) ;
#6199 = EDGE_LOOP ( 'NONE', ( #14419, #5510, #6824, #13769 ) ) ;
#6200 = ADVANCED_FACE ( 'NONE', ( #9716 ), #6259, .F. ) ;
#6201 = DIRECTION ( 'NONE',  ( 0.000000000000000000, 0.000000000000000000, -1.000000000000000000 ) ) ;
#6202 = EDGE_CURVE ( 'NONE', #8186, #12412, #7347, .T. ) ;
#6203 = CARTESIAN_POINT ( 'NONE',  ( -3.458861090693667872, -5.280908638085628937, 0.2950975219710819109 ) ) ;
#6204 = DIRECTION ( 'NONE',  ( 1.000000000000000000, 2.551930889570660354E-15, 0.000000000000000000 ) ) ;
#6205 = CARTESIAN_POINT ( 'NONE',  ( -1.006616814747114065E-29, -2.568816543514387226E-44, 0.000000000000000000 ) ) ;
#6206 = FACE_OUTER_BOUND ( 'NONE', #14515, .T. ) ;
#6207 = CARTESIAN_POINT ( 'NONE',  ( 21.98164641901421135, 11.39999970914575833, -0.3335879563140091153 ) ) ;
#6208 =( BOUNDED_CURVE ( )  B_SPLINE_CURVE ( 3, ( #11030, #3819, #10884, #9929 ),
 .UNSPECIFIED., .F., .T. ) 
 B_SPLINE_CURVE_WITH_KNOTS ( ( 4, 4 ),
 ( 4.207727487654162601, 4.529736049611353010 ),
 .UNSPECIFIED. ) 
 CURVE ( )  GEOMETRIC_REPRESENTATION_ITEM ( )  RATIONAL_B_SPLINE_CURVE ( ( 1.000000000000000000, 0.9913778568727538154, 0.9913778568727538154, 1.000000000000000000 ) ) 
 REPRESENTATION_ITEM ( '' )  );
#6209 = ORIENTED_EDGE ( 'NONE', *, *, #6528, .T. ) ;
#6210 = FACE_OUTER_BOUND ( 'NONE', #2024, .T. ) ;
#6211 = ORIENTED_EDGE ( 'NONE', *, *, #194, .T. ) ;
#6212 = DIRECTION ( 'NONE',  ( 0.000000000000000000, 0.000000000000000000, 1.000000000000000000 ) ) ;
#6213 = CARTESIAN_POINT ( 'NONE',  ( -0.6956252696767807331, -3.303750000000123421, 3.503916970779589413 ) ) ;
#6214 = ORIENTED_EDGE ( 'NONE', *, *, #7553, .F. ) ;
#6215 = ORIENTED_EDGE ( 'NONE', *, *, #8859, .T. ) ;
#6216 = EDGE_CURVE ( 'NONE', #3055, #382, #14761, .T. ) ;
#6217 = ORIENTED_EDGE ( 'NONE', *, *, #292, .F. ) ;
#6218 = CARTESIAN_POINT ( 'NONE',  ( -60.52799568714584666, 103.6741184958669919, -79.59847958357700293 ) ) ;
#6219 = EDGE_CURVE ( 'NONE', #1114, #3042, #1663, .T. ) ;
#6220 = CARTESIAN_POINT ( 'NONE',  ( -2.214775092167319492, -5.213036032544459353, -2.777127259766121181 ) ) ;
#6221 = DIRECTION ( 'NONE',  ( 0.000000000000000000, 0.000000000000000000, 1.000000000000000000 ) ) ;
#6222 = CARTESIAN_POINT ( 'NONE',  ( -3.525127887470900223, -0.4995676945082684339, -2.371274685879552369 ) ) ;
#6223 = DIRECTION ( 'NONE',  ( 0.000000000000000000, 1.000000000000000000, 4.336808689942017736E-16 ) ) ;
#6224 = CARTESIAN_POINT ( 'NONE',  ( -87.79538362643998539, 63.40569462133918677, -147.9984795835769944 ) ) ;
#6225 = EDGE_CURVE ( 'NONE', #7739, #13195, #11072, .T. ) ;
#6226 = ORIENTED_EDGE ( 'NONE', *, *, #5804, .F. ) ;
#6227 = LINE ( 'NONE', #10789, #11244 ) ;
#6228 = ORIENTED_EDGE ( 'NONE', *, *, #6501, .F. ) ;
#6229 = VERTEX_POINT ( 'NONE', #14679 ) ;
#6230 = VERTEX_POINT ( 'NONE', #11124 ) ;
#6231 = VERTEX_POINT ( 'NONE', #8792 ) ;
#6232 = EDGE_CURVE ( 'NONE', #5168, #557, #6412, .T. ) ;
#6233 = SPHERICAL_SURFACE ( 'NONE', #2579, 1.000000000000000000 ) ;
#6234 = CARTESIAN_POINT ( 'NONE',  ( -0.3703630857574056745, -1.850625000000086340, -3.746264557426716379 ) ) ;
#6235 = ADVANCED_FACE ( 'NONE', ( #5228 ), #1633, .T. ) ;
#6236 = EDGE_CURVE ( 'NONE', #12668, #4506, #1128, .T. ) ;
#6237 =( LENGTH_UNIT ( ) NAMED_UNIT ( * ) SI_UNIT ( .MILLI., .METRE. ) );
#6238 = CARTESIAN_POINT ( 'NONE',  ( -0.7718104722664602679, -3.281249999999995115, -3.872775259196827857 ) ) ;
#6239 = LINE ( 'NONE', #307, #14433 ) ;
#6240 = FACE_OUTER_BOUND ( 'NONE', #13158, .T. ) ;
#6241 = DIRECTION ( 'NONE',  ( -0.7071067811865474617, 8.659560562354921765E-17, 0.7071067811865474617 ) ) ;
#6242 = DIRECTION ( 'NONE',  ( 0.9961946980917452121, -3.779777825264104572E-17, 0.08715574274766174634 ) ) ;
#6243 = DIRECTION ( 'NONE',  ( -0.8660254037844385966, -2.210036979070412685E-15, 0.5000000000000003331 ) ) ;
#6244 = CARTESIAN_POINT ( 'NONE',  ( -48.27438362644000591, 65.17411849586700612, -86.49847958357699440 ) ) ;
#6245 = TOROIDAL_SURFACE ( 'NONE', #8196, 1.200000000000000178, 0.6000000000000000888 ) ;
#6246 = EDGE_CURVE ( 'NONE', #6301, #8515, #13610, .T. ) ;
#6247 = ORIENTED_EDGE ( 'NONE', *, *, #13341, .T. ) ;
#6248 = DIRECTION ( 'NONE',  ( 0.8660254037844387076, 0.4999999999999998890, 0.000000000000000000 ) ) ;
#6249 = VERTEX_POINT ( 'NONE', #12066 ) ;
#6250 = CIRCLE ( 'NONE', #14636, 1.500000000000001332 ) ;
#6251 = ORIENTED_EDGE ( 'NONE', *, *, #3947, .F. ) ;
#6252 = CARTESIAN_POINT ( 'NONE',  ( 0.3227798623957478519, -5.350624999999817888, 3.285751646651179581 ) ) ;
#6253 = EDGE_CURVE ( 'NONE', #11163, #12032, #1432, .T. ) ;
#6254 = DIRECTION ( 'NONE',  ( -1.460279444460352888E-17, 0.7071067811865485719, -0.7071067811865465735 ) ) ;
#6255 = CARTESIAN_POINT ( 'NONE',  ( 3.740778800480223154, -1.077338562373169495, -1.998207761774829949 ) ) ;
#6256 = CIRCLE ( 'NONE', #14884, 0.5999999999999998668 ) ;
#6257 = FACE_OUTER_BOUND ( 'NONE', #8167, .T. ) ;
#6258 = CARTESIAN_POINT ( 'NONE',  ( 57.41329019055577021, 5.000000000000001776, 129.5095611191910621 ) ) ;
#6259 = CYLINDRICAL_SURFACE ( 'NONE', #6614, 9.999999999999994671 ) ;
#6260 = AXIS2_PLACEMENT_3D ( 'NONE', #13149, #10646, #9556 ) ;
#6261 = CARTESIAN_POINT ( 'NONE',  ( -54.81638362644100226, 99.17411849586700612, -147.9984795835769944 ) ) ;
#6262 = DIRECTION ( 'NONE',  ( 0.8660254037844383745, -0.5000000000000003331, 0.000000000000000000 ) ) ;
#6263 = DIRECTION ( 'NONE',  ( 0.000000000000000000, 0.000000000000000000, 1.000000000000000000 ) ) ;
#6264 = ORIENTED_EDGE ( 'NONE', *, *, #13764, .F. ) ;
#6265 = AXIS2_PLACEMENT_3D ( 'NONE', #11792, #5918, #3565 ) ;
#6266 = ORIENTED_EDGE ( 'NONE', *, *, #14733, .F. ) ;
#6267 = CIRCLE ( 'NONE', #2034, 3.000000000000002665 ) ;
#6268 = DIRECTION ( 'NONE',  ( 0.000000000000000000, 0.000000000000000000, 1.000000000000000000 ) ) ;
#6269 = CARTESIAN_POINT ( 'NONE',  ( -2.938526230868574896, -4.390625000000237144, -2.412868667173103443 ) ) ;
#6270 = VERTEX_POINT ( 'NONE', #6188 ) ;
#6271 = AXIS2_PLACEMENT_3D ( 'NONE', #830, #12334, #1769 ) ;
#6272 = CARTESIAN_POINT ( 'NONE',  ( 0.001378637340237239689, -4.749213562373086894, 3.755245864738716577 ) ) ;
#6273 = CARTESIAN_POINT ( 'NONE',  ( 3.518605591592535387, -1.522500000000036380, 1.455944046807712278 ) ) ;
#6274 = CARTESIAN_POINT ( 'NONE',  ( 26.27204830164800953, -1.924145975121151140E-15, 27.91162381282022054 ) ) ;
#6275 = FACE_OUTER_BOUND ( 'NONE', #9977, .T. ) ;
#6276 = CARTESIAN_POINT ( 'NONE',  ( -77.52077156573416516, 164.3482369917340122, -73.34256232478206528 ) ) ;
#6277 = CARTESIAN_POINT ( 'NONE',  ( -15.50000000000000000, -2.500000000000000000, 23.94337567297399971 ) ) ;
#6278 = CARTESIAN_POINT ( 'NONE',  ( 1.947697749281812607, -5.403728638081555680, 2.678754459976768310 ) ) ;
#6279 = CARTESIAN_POINT ( 'NONE',  ( 0.000000000000000000, 0.000000000000000000, 6.000000000000000000 ) ) ;
#6280 = DIRECTION ( 'NONE',  ( -0.000000000000000000, -1.000000000000000000, -0.000000000000000000 ) ) ;
#6281 = DIRECTION ( 'NONE',  ( -0.000000000000000000, 1.000000000000000000, -0.000000000000000000 ) ) ;
#6282 = ORIENTED_EDGE ( 'NONE', *, *, #12466, .T. ) ;
#6283 = EDGE_LOOP ( 'NONE', ( #12201, #5048, #14797, #3361, #5132, #8090 ) ) ;
#6284 = DIRECTION ( 'NONE',  ( 1.000000000000000000, 0.000000000000000000, 0.000000000000000000 ) ) ;
#6285 = EDGE_CURVE ( 'NONE', #1774, #8449, #3616, .T. ) ;
#6286 = ORIENTED_EDGE ( 'NONE', *, *, #11774, .T. ) ;
#6287 = CIRCLE ( 'NONE', #15157, 3.300000002979700753 ) ;
#6288 = CARTESIAN_POINT ( 'NONE',  ( 17.18164641901421419, -11.40000029085424238, -0.3335879563140091153 ) ) ;
#6289 = CARTESIAN_POINT ( 'NONE',  ( -1.038475776471825984, -3.288125000000012843, 3.420226703972063298 ) ) ;
#6290 = VERTEX_POINT ( 'NONE', #12371 ) ;
#6291 = ORIENTED_EDGE ( 'NONE', *, *, #232, .F. ) ;
#6292 = DIRECTION ( 'NONE',  ( 1.000000000000000000, 0.000000000000000000, 0.000000000000000000 ) ) ;
#6293 = VECTOR ( 'NONE', #1720, 1000.000000000000000 ) ;
#6294 = CARTESIAN_POINT ( 'NONE',  ( -14.25000000000000000, -2.500000000000000000, 21.77831216351300014 ) ) ;
#6295 = CARTESIAN_POINT ( 'NONE',  ( 17.18164641901421419, 11.99999970914575798, -0.3335879563140091153 ) ) ;
#6296 = AXIS2_PLACEMENT_3D ( 'NONE', #13777, #1021, #3356 ) ;
#6297 = CARTESIAN_POINT ( 'NONE',  ( -1.254886650950876925, -0.4995676945082626608, -3.987764699483664188 ) ) ;
#6298 = CARTESIAN_POINT ( 'NONE',  ( -14.25000000000000000, -0.2038245569916330158, -21.77831216351300014 ) ) ;
#6299 = ADVANCED_FACE ( 'NONE', ( #13311 ), #7414, .T. ) ;
#6300 = CYLINDRICAL_SURFACE ( 'NONE', #7311, 3.499999999999999556 ) ;
#6301 = VERTEX_POINT ( 'NONE', #422 ) ;
#6302 = CARTESIAN_POINT ( 'NONE',  ( -15.08757311576351690, -0.3152598339557960427, 23.70526090033903444 ) ) ;
#6303 = AXIS2_PLACEMENT_3D ( 'NONE', #5329, #10042, #3561 ) ;
#6304 = EDGE_CURVE ( 'NONE', #7017, #384, #4874, .T. ) ;
#6305 = ORIENTED_EDGE ( 'NONE', *, *, #2486, .F. ) ;
#6306 = ORIENTED_EDGE ( 'NONE', *, *, #4575, .F. ) ;
#6307 = ORIENTED_EDGE ( 'NONE', *, *, #5753, .T. ) ;
#6308 = VERTEX_POINT ( 'NONE', #1583 ) ;
#6309 = VECTOR ( 'NONE', #7703, 1000.000000000000000 ) ;
#6310 = CARTESIAN_POINT ( 'NONE',  ( -48.27438362644000591, 65.17411849586700612, -86.49847958357699440 ) ) ;
#6311 = CARTESIAN_POINT ( 'NONE',  ( -0.3615547238505233407, -2.319374999999934239, 3.684823279838126187 ) ) ;
#6312 = CARTESIAN_POINT ( 'NONE',  ( -3.613419487966115895, -3.562500000000009326, 1.498272701152596031 ) ) ;
#6313 = CIRCLE ( 'NONE', #5806, 2.750000000000002665 ) ;
#6314 = PLANE ( 'NONE',  #12455 ) ;
#6315 = AXIS2_PLACEMENT_3D ( 'NONE', #11233, #5428, #826 ) ;
#6316 = DIRECTION ( 'NONE',  ( -2.551930889570659960E-15, 1.000000000000000000, 0.000000000000000000 ) ) ;
#6317 = DIRECTION ( 'NONE',  ( 1.000000000000000000, 0.000000000000000000, 0.000000000000000000 ) ) ;
#6318 = FACE_OUTER_BOUND ( 'NONE', #7419, .T. ) ;
#6319 = PLANE ( 'NONE',  #10266 ) ;
#6320 = EDGE_CURVE ( 'NONE', #12945, #9206, #5163, .T. ) ;
#6321 = CARTESIAN_POINT ( 'NONE',  ( 4.573385150445044900, -3.618985300545107364, 0.000000000000000000 ) ) ;
#6322 = CARTESIAN_POINT ( 'NONE',  ( -75.01311196519617397, 67.29799558322736175, -81.84847958357698872 ) ) ;
#6323 = VERTEX_POINT ( 'NONE', #865 ) ;
#6324 = DIRECTION ( 'NONE',  ( 0.000000000000000000, 1.000000000000000000, 0.000000000000000000 ) ) ;
#6325 = EDGE_CURVE ( 'NONE', #15063, #6954, #12598, .T. ) ;
#6326 = VERTEX_POINT ( 'NONE', #11276 ) ;
#6327 = ORIENTED_EDGE ( 'NONE', *, *, #10839, .T. ) ;
#6328 = ORIENTED_EDGE ( 'NONE', *, *, #8174, .T. ) ;
#6329 = CARTESIAN_POINT ( 'NONE',  ( -3.191126515704096001, -6.069374228118336490, -0.3131016245760978034 ) ) ;
#6330 = VECTOR ( 'NONE', #2235, 999.9999999999998863 ) ;
#6331 = AXIS2_PLACEMENT_3D ( 'NONE', #199, #9888, #2451 ) ;
#6332 = CYLINDRICAL_SURFACE ( 'NONE', #10690, 4.000000000000004441 ) ;
#6333 = CARTESIAN_POINT ( 'NONE',  ( -0.9755776780686565841, -4.881874999999863185, -3.218989981404408951 ) ) ;
#6334 = EDGE_CURVE ( 'NONE', #14279, #2123, #786, .T. ) ;
#6335 = FACE_BOUND ( 'NONE', #5679, .T. ) ;
#6336 = DIRECTION ( 'NONE',  ( 1.000000000000000000, 0.000000000000000000, 0.000000000000000000 ) ) ;
#6337 = CARTESIAN_POINT ( 'NONE',  ( -15.50000000000000000, -1.037157890325000054, 19.00000000000000000 ) ) ;
#6338 = LINE ( 'NONE', #11125, #5158 ) ;
#6339 = DIRECTION ( 'NONE',  ( 1.000000000000000000, 0.000000000000000000, 0.000000000000000000 ) ) ;
#6340 = ADVANCED_FACE ( 'NONE', ( #12440 ), #3271, .F. ) ;
#6341 = DIRECTION ( 'NONE',  ( -1.000000000000000000, 0.000000000000000000, 0.000000000000000000 ) ) ;
#6342 = EDGE_LOOP ( 'NONE', ( #9385, #12705, #11641, #13947 ) ) ;
#6343 = AXIS2_PLACEMENT_3D ( 'NONE', #11736, #5858, #12984 ) ;
#6344 = DIRECTION ( 'NONE',  ( 0.000000000000000000, -1.000000000000000000, 0.000000000000000000 ) ) ;
#6345 = EDGE_CURVE ( 'NONE', #8406, #11643, #13272, .T. ) ;
#6346 = EDGE_CURVE ( 'NONE', #12791, #11451, #9560, .T. ) ;
#6347 = ORIENTED_EDGE ( 'NONE', *, *, #13550, .F. ) ;
#6348 = PRODUCT_DEFINITION_SHAPE ( 'NONE', 'NONE',  #15344 ) ;
#6349 = LINE ( 'NONE', #6421, #4859 ) ;
#6350 = CARTESIAN_POINT ( 'NONE',  ( 3.506874188274308413, -3.078124999999926281, -1.873277435140577429 ) ) ;
#6351 = EDGE_LOOP ( 'NONE', ( #10902, #9877, #6264, #3419 ) ) ;
#6352 = CIRCLE ( 'NONE', #11529, 2.750000000000002665 ) ;
#6353 = AXIS2_PLACEMENT_3D ( 'NONE', #8361, #9195, #11619 ) ;
#6354 = DIRECTION ( 'NONE',  ( 0.000000000000000000, 0.000000000000000000, 1.000000000000000000 ) ) ;
#6355 = CARTESIAN_POINT ( 'NONE',  ( 17.04394838817069413, 11.39999970914576011, 0.2824263826447109826 ) ) ;
#6356 = DIRECTION ( 'NONE',  ( 0.000000000000000000, 0.000000000000000000, -1.000000000000000000 ) ) ;
#6357 = LINE ( 'NONE', #9820, #14591 ) ;
#6358 = CARTESIAN_POINT ( 'NONE',  ( -88.81638362644000040, 66.35306774555222376, -147.9984795835769944 ) ) ;
#6359 = FACE_OUTER_BOUND ( 'NONE', #3886, .T. ) ;
#6360 = AXIS2_PLACEMENT_3D ( 'NONE', #12049, #14434, #7402 ) ;
#6361 = CARTESIAN_POINT ( 'NONE',  ( -0.8000000000000178080, 9.500000000000000000, 0.000000000000000000 ) ) ;
#6362 = VECTOR ( 'NONE', #8254, 1000.000000000000000 ) ;
#6363 = AXIS2_PLACEMENT_3D ( 'NONE', #8832, #5355, #829 ) ;
#6364 = ORIENTED_EDGE ( 'NONE', *, *, #12670, .T. ) ;
#6365 = ORIENTED_EDGE ( 'NONE', *, *, #4996, .T. ) ;
#6366 = CARTESIAN_POINT ( 'NONE',  ( 3.341236413112297576, -1.663124999999897824, -1.787503410618120236 ) ) ;
#6367 = ORIENTED_EDGE ( 'NONE', *, *, #14970, .F. ) ;
#6368 = CONICAL_SURFACE ( 'NONE', #13305, 3.749999999999996447, 0.7853981633974476129 ) ;
#6369 = DIRECTION ( 'NONE',  ( -1.000000000000000000, 0.000000000000000000, 0.000000000000000000 ) ) ;
#6370 = AXIS2_PLACEMENT_3D ( 'NONE', #9692, #9854, #12269 ) ;
#6371 = CIRCLE ( 'NONE', #7351, 2.042000000000002036 ) ;
#6372 = CARTESIAN_POINT ( 'NONE',  ( 3.897114317029974018, 9.945166405816858860E-15, -2.250000000000001332 ) ) ;
#6373 = CARTESIAN_POINT ( 'NONE',  ( -90.85838362644101096, 99.17411849586700612, -147.9984795835769944 ) ) ;
#6374 = CARTESIAN_POINT ( 'NONE',  ( -3.979857382319186510, -0.4995676945082694886, -1.548798448790204452 ) ) ;
#6375 =( NAMED_UNIT ( * ) PLANE_ANGLE_UNIT ( ) SI_UNIT ( $, .RADIAN. ) );
#6376 = DIRECTION ( 'NONE',  ( 1.060575238724892987E-16, 0.5000000000000199840, -0.8660254037844271613 ) ) ;
#6377 = ORIENTED_EDGE ( 'NONE', *, *, #2848, .F. ) ;
#6378 = FACE_BOUND ( 'NONE', #8683, .T. ) ;
#6379 = EDGE_LOOP ( 'NONE', ( #14462, #628, #820, #12603 ) ) ;
#6380 = AXIS2_PLACEMENT_3D ( 'NONE', #3644, #3406, #13117 ) ;
#6381 = ORIENTED_EDGE ( 'NONE', *, *, #2887, .F. ) ;
#6382 = ORIENTED_EDGE ( 'NONE', *, *, #6592, .F. ) ;
#6383 = ORIENTED_EDGE ( 'NONE', *, *, #14970, .T. ) ;
#6384 = EDGE_LOOP ( 'NONE', ( #13853, #14704, #4189, #7942 ) ) ;
#6385 = DIRECTION ( 'NONE',  ( -1.000000000000000000, 0.000000000000000000, 0.000000000000000000 ) ) ;
#6386 = ADVANCED_FACE ( 'NONE', ( #10398 ), #10098, .F. ) ;
#6387 = CARTESIAN_POINT ( 'NONE',  ( 0.3615547238501363725, -2.350625000000046150, 3.680709139401309837 ) ) ;
#6388 = CARTESIAN_POINT ( 'NONE',  ( -1.780457766239074071E-14, 9.500000000000000000, 6.182228413854880884E-29 ) ) ;
#6389 = AXIS2_PLACEMENT_3D ( 'NONE', #8549, #7174, #14437 ) ;
#6390 = CARTESIAN_POINT ( 'NONE',  ( -3.630950894689927821, -4.453124999999883649, -1.099983568547476143 ) ) ;
#6391 = CARTESIAN_POINT ( 'NONE',  ( -61.72438362644000165, 82.17411849586700612, -85.04847958357699156 ) ) ;
#6392 = ADVANCED_FACE ( 'NONE', ( #13901 ), #4368, .F. ) ;
#6393 = CARTESIAN_POINT ( 'NONE',  ( -46.58670980944423690, 5.000000000000000000, 135.5095611191910621 ) ) ;
#6394 = VECTOR ( 'NONE', #13792, 1000.000000000000114 ) ;
#6395 = DIRECTION ( 'NONE',  ( 0.000000000000000000, 0.000000000000000000, 1.000000000000000000 ) ) ;
#6396 = CARTESIAN_POINT ( 'NONE',  ( 15.50000000000000000, -0.1999999999999999556, -22.50000000000000000 ) ) ;
#6397 = DIRECTION ( 'NONE',  ( 0.08715574274766167695, 0.000000000000000000, -0.9961946980917453232 ) ) ;
#6398 = LINE ( 'NONE', #14816, #1403 ) ;
#6399 = DIRECTION ( 'NONE',  ( 0.000000000000000000, 0.000000000000000000, 1.000000000000000000 ) ) ;
#6400 = ORIENTED_EDGE ( 'NONE', *, *, #136, .F. ) ;
#6401 = CARTESIAN_POINT ( 'NONE',  ( 23.25000000000000000, 0.000000000000000000, 27.00000000000000000 ) ) ;
#6402 = ORIENTED_EDGE ( 'NONE', *, *, #8077, .T. ) ;
#6403 = VERTEX_POINT ( 'NONE', #5545 ) ;
#6404 = ORIENTED_EDGE ( 'NONE', *, *, #13896, .F. ) ;
#6405 = CARTESIAN_POINT ( 'NONE',  ( 2.325173090398219067, -5.459999999999847198, 2.323431042901937360 ) ) ;
#6406 = CIRCLE ( 'NONE', #15037, 4.250000000000003553 ) ;
#6407 = DIRECTION ( 'NONE',  ( -0.000000000000000000, 1.000000000000000000, -0.000000000000000000 ) ) ;
#6408 = EDGE_CURVE ( 'NONE', #12872, #7767, #13554, .T. ) ;
#6409 = CARTESIAN_POINT ( 'NONE',  ( 2.325173090398219067, -5.459999999999847198, 2.323431042901936916 ) ) ;
#6410 = CARTESIAN_POINT ( 'NONE',  ( -13.41835358098578723, -11.40000029085424238, -0.3335879563140091153 ) ) ;
#6411 = CARTESIAN_POINT ( 'NONE',  ( -69.77438362644001302, 82.17411849586700612, -80.44847958357698303 ) ) ;
#6412 = LINE ( 'NONE', #12137, #10549 ) ;
#6413 = DIRECTION ( 'NONE',  ( 0.000000000000000000, 0.000000000000000000, -1.000000000000000000 ) ) ;
#6414 = DIRECTION ( 'NONE',  ( 0.000000000000000000, 0.000000000000000000, 1.000000000000000000 ) ) ;
#6415 = DIRECTION ( 'NONE',  ( 0.08715574274766167695, 0.000000000000000000, -0.9961946980917453232 ) ) ;
#6416 = ORIENTED_EDGE ( 'NONE', *, *, #5058, .F. ) ;
#6417 = CARTESIAN_POINT ( 'NONE',  ( 15.29633693294940500, -0.2717122460100945269, 23.82579074638835692 ) ) ;
#6418 = EDGE_CURVE ( 'NONE', #9995, #3958, #12062, .T. ) ;
#6419 = EDGE_CURVE ( 'NONE', #13943, #5822, #5382, .T. ) ;
#6420 = ORIENTED_EDGE ( 'NONE', *, *, #14794, .T. ) ;
#6421 = CARTESIAN_POINT ( 'NONE',  ( -56.52438362644099357, 99.17411849586700612, -150.4984795835770228 ) ) ;
#6422 = CARTESIAN_POINT ( 'NONE',  ( 4.096389842826703820, -2.015625000000050182, -0.4049582849837481402 ) ) ;
#6423 = EDGE_LOOP ( 'NONE', ( #3709, #13982, #10551, #1256 ) ) ;
#6424 = EDGE_CURVE ( 'NONE', #486, #14010, #12522, .T. ) ;
#6425 = CONICAL_SURFACE ( 'NONE', #13105, 3.637955631634646192, 0.1308996938995775905 ) ;
#6426 = CYLINDRICAL_SURFACE ( 'NONE', #2002, 2.750000000000002665 ) ;
#6427 = EDGE_CURVE ( 'NONE', #558, #14943, #1884, .T. ) ;
#6428 = FACE_OUTER_BOUND ( 'NONE', #14027, .T. ) ;
#6429 = EDGE_CURVE ( 'NONE', #9368, #9847, #14276, .T. ) ;
#6430 = DIRECTION ( 'NONE',  ( 0.000000000000000000, 0.000000000000000000, 1.000000000000000000 ) ) ;
#6431 = FACE_OUTER_BOUND ( 'NONE', #14196, .T. ) ;
#6432 = CARTESIAN_POINT ( 'NONE',  ( -86.77438362643999881, 65.17411849586700612, -147.9984795835769944 ) ) ;
#6433 = DIRECTION ( 'NONE',  ( 1.000000000000000000, 8.284258017326334836E-16, 0.000000000000000000 ) ) ;
#6434 = CARTESIAN_POINT ( 'NONE',  ( -69.77438362644001302, 82.17411849586700612, -43.99847958362880007 ) ) ;
#6435 = DIRECTION ( 'NONE',  ( -1.000000000000000000, 0.000000000000000000, 0.000000000000000000 ) ) ;
#6436 = CONICAL_SURFACE ( 'NONE', #12127, 4.500000000000000888, 1.396263401595466691 ) ;
#6437 = EDGE_CURVE ( 'NONE', #13375, #15273, #156, .T. ) ;
#6438 = ORIENTED_EDGE ( 'NONE', *, *, #14711, .F. ) ;
#6439 =( NAMED_UNIT ( * ) PLANE_ANGLE_UNIT ( ) SI_UNIT ( $, .RADIAN. ) );
#6440 = ORIENTED_EDGE ( 'NONE', *, *, #3757, .T. ) ;
#6441 = DIRECTION ( 'NONE',  ( -9.422394424380274864E-16, 1.000000000000000000, -0.000000000000000000 ) ) ;
#6442 = CARTESIAN_POINT ( 'NONE',  ( -1.418005212499603429, -2.272500000000021281, 3.426931839692804793 ) ) ;
#6443 = ORIENTED_EDGE ( 'NONE', *, *, #9530, .T. ) ;
#6444 = EDGE_CURVE ( 'NONE', #6610, #4486, #6858, .T. ) ;
#6445 = DIRECTION ( 'NONE',  ( 0.000000000000000000, 0.000000000000000000, 1.000000000000000000 ) ) ;
#6446 = CARTESIAN_POINT ( 'NONE',  ( 1.233021357193251788, -0.4995676945082553888, -3.929992886820973474 ) ) ;
#6447 = DIRECTION ( 'NONE',  ( 0.000000000000000000, 0.000000000000000000, 1.000000000000000000 ) ) ;
#6448 = FACE_OUTER_BOUND ( 'NONE', #4113, .T. ) ;
#6449 = LINE ( 'NONE', #9987, #12749 ) ;
#6450 = VERTEX_POINT ( 'NONE', #5466 ) ;
#6451 = CARTESIAN_POINT ( 'NONE',  ( -86.77438362644100778, 99.17411849586700612, -147.9984795835769944 ) ) ;
#6452 = ORIENTED_EDGE ( 'NONE', *, *, #13628, .F. ) ;
#6453 = PRODUCT_DEFINITION_FORMATION_WITH_SPECIFIED_SOURCE ( 'ANY', '', #9435, .NOT_KNOWN. ) ;
#6454 = EDGE_LOOP ( 'NONE', ( #710, #10372, #294, #11874 ) ) ;
#6455 = ORIENTED_EDGE ( 'NONE', *, *, #615, .T. ) ;
#6456 = ORIENTED_EDGE ( 'NONE', *, *, #9705, .F. ) ;
#6457 = ORIENTED_EDGE ( 'NONE', *, *, #7891, .T. ) ;
#6458 = DIRECTION ( 'NONE',  ( -1.000000000000000000, 1.734723475976808475E-15, 0.000000000000000000 ) ) ;
#6459 = CARTESIAN_POINT ( 'NONE',  ( 3.518605591592535387, -1.522500000000036380, 1.455944046807712278 ) ) ;
#6460 = FACE_BOUND ( 'NONE', #7446, .T. ) ;
#6461 = CARTESIAN_POINT ( 'NONE',  ( 2.130457310823663519, -4.156249999999911182, -3.186652721750134809 ) ) ;
#6462 = DIRECTION ( 'NONE',  ( 0.000000000000000000, 0.000000000000000000, -1.000000000000000000 ) ) ;
#6463 = CARTESIAN_POINT ( 'NONE',  ( -52.77438362643999881, 65.17411849586700612, -182.2484795835770228 ) ) ;
#6464 = CARTESIAN_POINT ( 'NONE',  ( 22.58164641901421632, 12.49999970914576153, -8.775548064764198131 ) ) ;
#6465 = CARTESIAN_POINT ( 'NONE',  ( 1.227202584385329587, -1.203124999999989342, -4.041673972266214498 ) ) ;
#6466 = CARTESIAN_POINT ( 'NONE',  ( 16.75000000000000000, -0.2038245569916320166, 21.77831216351300014 ) ) ;
#6467 = CARTESIAN_POINT ( 'NONE',  ( -15.50000000000000000, -0.1999999999999999556, 21.05000000000000071 ) ) ;
#6468 = DIRECTION ( 'NONE',  ( 1.000000000000000000, 0.000000000000000000, 0.000000000000000000 ) ) ;
#6469 = VERTEX_POINT ( 'NONE', #10163 ) ;
#6470 = DIRECTION ( 'NONE',  ( 1.000000000000000000, 0.000000000000000000, -6.982962677686266711E-15 ) ) ;
#6471 = VERTEX_POINT ( 'NONE', #14898 ) ;
#6472 = ORIENTED_EDGE ( 'NONE', *, *, #214, .T. ) ;
#6473 = VERTEX_POINT ( 'NONE', #5625 ) ;
#6474 = PLANE ( 'NONE',  #2022 ) ;
#6475 = EDGE_CURVE ( 'NONE', #13765, #1201, #9015, .T. ) ;
#6476 = DIRECTION ( 'NONE',  ( 0.000000000000000000, 0.000000000000000000, -1.000000000000000000 ) ) ;
#6477 = FACE_OUTER_BOUND ( 'NONE', #9592, .T. ) ;
#6478 = DIRECTION ( 'NONE',  ( 0.000000000000000000, -0.000000000000000000, 1.000000000000000000 ) ) ;
#6479 = DIRECTION ( 'NONE',  ( 0.000000000000000000, 1.000000000000000000, 0.000000000000000000 ) ) ;
#6480 = CARTESIAN_POINT ( 'NONE',  ( -75.01311196519617397, 67.29799558322736175, -83.44847958357698303 ) ) ;
#6481 = CARTESIAN_POINT ( 'NONE',  ( 57.41329019055577021, 0.000000000000000000, 129.5095611191910621 ) ) ;
#6482 = VECTOR ( 'NONE', #2704, 1000.000000000000000 ) ;
#6483 = CARTESIAN_POINT ( 'NONE',  ( 2.393563981450126388, -4.710000000000058584, -2.395350030107596506 ) ) ;
#6484 = ORIENTED_EDGE ( 'NONE', *, *, #14162, .F. ) ;
#6485 = DIRECTION ( 'NONE',  ( 1.000000000000000000, 0.000000000000000000, 0.000000000000000000 ) ) ;
#6486 = ADVANCED_FACE ( 'NONE', ( #6709 ), #3500, .F. ) ;
#6487 = ORIENTED_EDGE ( 'NONE', *, *, #6805, .F. ) ;
#6488 = ADVANCED_FACE ( 'NONE', ( #4594 ), #7165, .F. ) ;
#6489 = AXIS2_PLACEMENT_3D ( 'NONE', #11136, #2920, #1743 ) ;
#6490 = CARTESIAN_POINT ( 'NONE',  ( -4.030856054181176873, -2.515624999999848121, 0.3959303163381804880 ) ) ;
#6491 = EDGE_LOOP ( 'NONE', ( #5088, #8115, #11405, #13410 ) ) ;
#6492 = AXIS2_PLACEMENT_3D ( 'NONE', #11043, #3907, #4211 ) ;
#6493 = CARTESIAN_POINT ( 'NONE',  ( -84.27438362643998460, 65.17411849586700612, -79.59847958357700293 ) ) ;
#6494 = CARTESIAN_POINT ( 'NONE',  ( -15.50000000000000000, 0.000000000000000000, -18.50000000000000000 ) ) ;
#6495 = CARTESIAN_POINT ( 'NONE',  ( -86.77438362644001302, 59.67411849586700612, -152.4984795835769944 ) ) ;
#6496 = AXIS2_PLACEMENT_3D ( 'NONE', #4930, #10819, #10968 ) ;
#6497 = DIRECTION ( 'NONE',  ( -2.551930889570659960E-15, 1.000000000000000000, 0.000000000000000000 ) ) ;
#6498 = DIRECTION ( 'NONE',  ( -1.000000000000000000, 0.000000000000000000, 0.000000000000000000 ) ) ;
#6499 = DIRECTION ( 'NONE',  ( 0.000000000000000000, 4.336808689942017736E-16, -1.000000000000000000 ) ) ;
#6500 = DIRECTION ( 'NONE',  ( 0.000000000000000000, 0.000000000000000000, 1.000000000000000000 ) ) ;
#6501 = EDGE_CURVE ( 'NONE', #14030, #10998, #7091, .T. ) ;
#6502 = CARTESIAN_POINT ( 'NONE',  ( -50.02438362644000591, 65.17411849586700612, -145.4984795835769944 ) ) ;
#6503 = ORIENTED_EDGE ( 'NONE', *, *, #11722, .F. ) ;
#6504 = VECTOR ( 'NONE', #11239, 1000.000000000000114 ) ;
#6505 = VERTEX_POINT ( 'NONE', #1327 ) ;
#6506 = EDGE_CURVE ( 'NONE', #9953, #6629, #6090, .T. ) ;
#6507 = DIRECTION ( 'NONE',  ( 1.287488025362404182E-15, 1.000000000000000000, 0.000000000000000000 ) ) ;
#6508 = EDGE_CURVE ( 'NONE', #5722, #5825, #7357, .T. ) ;
#6509 = CARTESIAN_POINT ( 'NONE',  ( -3.795858268372354960, -1.053749999999936460, -0.7536008350790910360 ) ) ;
#6510 = EDGE_LOOP ( 'NONE', ( #7462, #3224, #3193, #9184 ) ) ;
#6511 = AXIS2_PLACEMENT_3D ( 'NONE', #3410, #8219, #10539 ) ;
#6512 = LINE ( 'NONE', #13572, #10675 ) ;
#6513 = EDGE_CURVE ( 'NONE', #14415, #59, #13136, .T. ) ;
#6514 = DIRECTION ( 'NONE',  ( 0.000000000000000000, 0.000000000000000000, 1.000000000000000000 ) ) ;
#6515 = VECTOR ( 'NONE', #10558, 1000.000000000000000 ) ;
#6516 = DIRECTION ( 'NONE',  ( -1.000000000000000000, 0.000000000000000000, 0.000000000000000000 ) ) ;
#6517 = CYLINDRICAL_SURFACE ( 'NONE', #4180, 4.500000000000003553 ) ;
#6518 = LINE ( 'NONE', #10205, #3282 ) ;
#6519 = CARTESIAN_POINT ( 'NONE',  ( 21.98164641901421135, 3.654316742536408924, 0.2664120436859909735 ) ) ;
#6520 = EDGE_CURVE ( 'NONE', #11928, #14868, #7006, .T. ) ;
#6521 = CARTESIAN_POINT ( 'NONE',  ( -54.81638362644100226, 97.99516924618178848, -147.9984795835769944 ) ) ;
#6522 = MECHANICAL_DESIGN_GEOMETRIC_PRESENTATION_REPRESENTATION (  '', ( #8488 ), #13455 ) ;
#6523 = ORIENTED_EDGE ( 'NONE', *, *, #792, .T. ) ;
#6524 = LINE ( 'NONE', #3094, #8758 ) ;
#6525 = ORIENTED_EDGE ( 'NONE', *, *, #9766, .T. ) ;
#6526 = EDGE_CURVE ( 'NONE', #7439, #1421, #14525, .T. ) ;
#6527 = VERTEX_POINT ( 'NONE', #167 ) ;
#6528 = EDGE_CURVE ( 'NONE', #1408, #13195, #4914, .T. ) ;
#6529 = EDGE_LOOP ( 'NONE', ( #1704, #5821, #606, #7856 ) ) ;
#6530 = EDGE_LOOP ( 'NONE', ( #386, #9749, #7691, #750 ) ) ;
#6531 = CIRCLE ( 'NONE', #4532, 3.000000000000002665 ) ;
#6532 = EDGE_LOOP ( 'NONE', ( #13749, #3169 ) ) ;
#6533 = DIRECTION ( 'NONE',  ( 1.000000000000000000, 0.000000000000000000, 0.000000000000000000 ) ) ;
#6534 = B_SPLINE_CURVE_WITH_KNOTS ( 'NONE', 3,
 ( #2282, #9265, #11672, #14230, #4625, #1041 ),
 .UNSPECIFIED., .F., .F.,
 ( 4, 2, 4 ),
 ( 0.000000000000000000, 0.001172976575130644768, 0.002345953150261289536 ),
 .UNSPECIFIED. ) ;
#6535 = AXIS2_PLACEMENT_3D ( 'NONE', #3072, #10044, #12318 ) ;
#6536 =( NAMED_UNIT ( * ) PLANE_ANGLE_UNIT ( ) SI_UNIT ( $, .RADIAN. ) );
#6537 = CARTESIAN_POINT ( 'NONE',  ( 3.553279128418493915, -4.062500000000332179, -1.470728592776388455 ) ) ;
#6538 = CARTESIAN_POINT ( 'NONE',  ( 4.573385150445044900, -3.618985300545107364, 6.000000000000000000 ) ) ;
#6539 = DIRECTION ( 'NONE',  ( 0.000000000000000000, 0.000000000000000000, -1.000000000000000000 ) ) ;
#6540 = CARTESIAN_POINT ( 'NONE',  ( -86.77438362644100778, 99.17411849586700612, -145.4984795835769944 ) ) ;
#6541 = CARTESIAN_POINT ( 'NONE',  ( 0.001544386136394801726, -0.7500000000000344169, 4.283781196144704317 ) ) ;
#6542 = DIRECTION ( 'NONE',  ( 0.4999999999999998890, -0.8660254037844387076, 0.000000000000000000 ) ) ;
#6543 = CARTESIAN_POINT ( 'NONE',  ( -69.77438362644001302, 82.17411849586700612, -43.99847958357699440 ) ) ;
#6544 = AXIS2_PLACEMENT_3D ( 'NONE', #5838, #4667, #7457 ) ;
#6545 = CARTESIAN_POINT ( 'NONE',  ( -15.50000000000000000, -0.1999999999999999556, -21.05000000000000071 ) ) ;
#6546 = ORIENTED_EDGE ( 'NONE', *, *, #10366, .T. ) ;
#6547 = CARTESIAN_POINT ( 'NONE',  ( 22.58164641901421632, -12.00000029085424025, -8.183940086454239093 ) ) ;
#6548 = ORIENTED_EDGE ( 'NONE', *, *, #689, .T. ) ;
#6549 = VECTOR ( 'NONE', #2781, 1000.000000000000000 ) ;
#6550 = VERTEX_POINT ( 'NONE', #11883 ) ;
#6551 = EDGE_LOOP ( 'NONE', ( #7992, #7689, #9098, #14950, #14046, #5635 ) ) ;
#6552 = UNCERTAINTY_MEASURE_WITH_UNIT (LENGTH_MEASURE( 1.000000000000000082E-05 ), #10749, 'distance_accuracy_value', 'NONE');
#6553 = CARTESIAN_POINT ( 'NONE',  ( -96.77438362643999881, 104.6741184958670061, -152.4984795835769944 ) ) ;
#6554 = CIRCLE ( 'NONE', #3069, 3.499999999999999556 ) ;
#6555 = CARTESIAN_POINT ( 'NONE',  ( -2.763334307196396722, -5.178749999999838316, 1.847896475581856324 ) ) ;
#6556 = AXIS2_PLACEMENT_3D ( 'NONE', #466, #11162, #2945 ) ;
#6557 = CARTESIAN_POINT ( 'NONE',  ( -52.77438362644100067, 96.81621999649657084, -147.9984795835769944 ) ) ;
#6558 = FACE_OUTER_BOUND ( 'NONE', #9458, .T. ) ;
#6559 = DIRECTION ( 'NONE',  ( -1.000000000000000000, 0.000000000000000000, 0.000000000000000000 ) ) ;
#6560 = DIRECTION ( 'NONE',  ( 0.000000000000000000, -0.000000000000000000, 1.000000000000000000 ) ) ;
#6561 = DIRECTION ( 'NONE',  ( 0.000000000000000000, 0.000000000000000000, -1.000000000000000000 ) ) ;
#6562 = CARTESIAN_POINT ( 'NONE',  ( 16.75000000000000000, -2.500000000000000000, 21.77831216351300014 ) ) ;
#6563 = VERTEX_POINT ( 'NONE', #11733 ) ;
#6564 = DIRECTION ( 'NONE',  ( 0.5000000000000003331, 0.8660254037844384856, 0.000000000000000000 ) ) ;
#6565 = VECTOR ( 'NONE', #8845, 1000.000000000000000 ) ;
#6566 = AXIS2_PLACEMENT_3D ( 'NONE', #4020, #12025, #9670 ) ;
#6567 = ORIENTED_EDGE ( 'NONE', *, *, #7434, .F. ) ;
#6568 = ITEM_DEFINED_TRANSFORMATION ( 'NONE', 'NONE', #7007,  #285 ) ;
#6569 = ORIENTED_EDGE ( 'NONE', *, *, #15102, .F. ) ;
#6570 = CARTESIAN_POINT ( 'NONE',  ( 3.434081308463064364, -1.906250000000116795, 2.295896066549416581 ) ) ;
#6571 = VERTEX_POINT ( 'NONE', #8394 ) ;
#6572 = CARTESIAN_POINT ( 'NONE',  ( -12.81835358098578403, 12.59999970914575940, -8.183940086454237317 ) ) ;
#6573 = AXIS2_PLACEMENT_3D ( 'NONE', #13193, #9839, #2553 ) ;
#6574 = ADVANCED_FACE ( 'NONE', ( #5772 ), #9622, .F. ) ;
#6575 = VECTOR ( 'NONE', #5776, 1000.000000000000000 ) ;
#6576 = DIRECTION ( 'NONE',  ( 0.000000000000000000, 0.000000000000000000, -1.000000000000000000 ) ) ;
#6577 = CARTESIAN_POINT ( 'NONE',  ( -52.77438362643999881, 67.53201699523744139, -147.9984795835769944 ) ) ;
#6578 = EDGE_CURVE ( 'NONE', #1067, #3159, #8826, .T. ) ;
#6579 = DIRECTION ( 'NONE',  ( -1.000000000000000000, 0.000000000000000000, 0.000000000000000000 ) ) ;
#6580 = CARTESIAN_POINT ( 'NONE',  ( -52.77438362644000591, 65.17411849586700612, -145.4984795835769660 ) ) ;
#6581 = LINE ( 'NONE', #14924, #10552 ) ;
#6582 = CARTESIAN_POINT ( 'NONE',  ( -66.83542154218349651, 97.90336940298355728, -93.68950033318012061 ) ) ;
#6583 = CARTESIAN_POINT ( 'NONE',  ( -75.01311196519617397, 67.29799558322736175, -83.44847958357698303 ) ) ;
#6584 = DIRECTION ( 'NONE',  ( 1.000000000000000000, 0.000000000000000000, 0.000000000000000000 ) ) ;
#6585 = ORIENTED_EDGE ( 'NONE', *, *, #14629, .T. ) ;
#6586 =( GEOMETRIC_REPRESENTATION_CONTEXT ( 3 ) GLOBAL_UNCERTAINTY_ASSIGNED_CONTEXT ( ( #2025 ) ) GLOBAL_UNIT_ASSIGNED_CONTEXT ( ( #8770, #2797, #395 ) ) REPRESENTATION_CONTEXT ( 'NONE', 'WORKASPACE' ) );
#6587 = DIRECTION ( 'NONE',  ( 1.000000000000000000, 0.000000000000000000, 0.000000000000000000 ) ) ;
#6588 = CARTESIAN_POINT ( 'NONE',  ( -2.355664480073799805, -2.225624999999979092, 2.872538697791624962 ) ) ;
#6589 = ORIENTED_EDGE ( 'NONE', *, *, #9901, .T. ) ;
#6590 = AXIS2_PLACEMENT_3D ( 'NONE', #14814, #6542, #5607 ) ;
#6591 = DIRECTION ( 'NONE',  ( 0.000000000000000000, 0.000000000000000000, 1.000000000000000000 ) ) ;
#6592 = EDGE_CURVE ( 'NONE', #1912, #10774, #5122, .T. ) ;
#6593 = PRESENTATION_LAYER_ASSIGNMENT (  '', '', ( #374 ) ) ;
#6594 = LINE ( 'NONE', #13862, #5819 ) ;
#6595 = ADVANCED_FACE ( 'NONE', ( #10635 ), #2487, .T. ) ;
#6596 = MECHANICAL_DESIGN_GEOMETRIC_PRESENTATION_REPRESENTATION (  '', ( #11288 ), #3862 ) ;
#6597 = CARTESIAN_POINT ( 'NONE',  ( 3.542101689960518662, -0.4995676945082338505, 1.737881650567584924 ) ) ;
#6598 = FILL_AREA_STYLE ('',( #12406 ) ) ;
#6599 = VECTOR ( 'NONE', #7382, 1000.000000000000114 ) ;
#6600 = DIRECTION ( 'NONE',  ( -0.8660254037844482555, 0.000000000000000000, 0.4999999999999831801 ) ) ;
#6601 = CARTESIAN_POINT ( 'NONE',  ( 16.12213235758455809, 11.99999970914575798, 0.3029999356681916667 ) ) ;
#6602 = ORIENTED_EDGE ( 'NONE', *, *, #14758, .T. ) ;
#6603 = CARTESIAN_POINT ( 'NONE',  ( -9.503456061879925088, 11.99999970914574021, 69.60114695342350899 ) ) ;
#6604 = VERTEX_POINT ( 'NONE', #12821 ) ;
#6605 = ADVANCED_FACE ( 'NONE', ( #8 ), #9465, .F. ) ;
#6606 = ORIENTED_EDGE ( 'NONE', *, *, #6151, .T. ) ;
#6607 = ORIENTED_EDGE ( 'NONE', *, *, #9833, .F. ) ;
#6608 = EDGE_CURVE ( 'NONE', #5090, #12114, #3586, .T. ) ;
#6609 = STYLED_ITEM ( 'NONE', ( #7424 ), #442 ) ;
#6610 = VERTEX_POINT ( 'NONE', #9393 ) ;
#6611 = B_SPLINE_CURVE_WITH_KNOTS ( 'NONE', 3,
 ( #11332, #7473, #4047, #3032, #549, #12507, #10081, #10010, #14586, #12190, #3966, #699 ),
 .UNSPECIFIED., .F., .F.,
 ( 4, 2, 2, 2, 2, 4 ),
 ( 2.544323688695237330E-07, 0.001342108318545689885, 0.002013035261634099626, 0.002683962204722509584, 0.004025816090899331234, 0.005367669977076151150 ),
 .UNSPECIFIED. ) ;
#6612 = ORIENTED_EDGE ( 'NONE', *, *, #1662, .F. ) ;
#6613 = SHAPE_REPRESENTATION ( 'Part2', ( #285 ), #1033 ) ;
#6614 = AXIS2_PLACEMENT_3D ( 'NONE', #13460, #255, #6479 ) ;
#6615 = CARTESIAN_POINT ( 'NONE',  ( -80.52077156573417938, 110.1741184958670061, -79.59847958357700293 ) ) ;
#6616 = AXIS2_PLACEMENT_3D ( 'NONE', #10599, #9428, #14244 ) ;
#6617 = CARTESIAN_POINT ( 'NONE',  ( 2.507317702870323739, -0.4443749999999629940, 3.052905756198839970 ) ) ;
#6618 = ADVANCED_FACE ( 'NONE', ( #9318 ), #14060, .F. ) ;
#6619 = CYLINDRICAL_SURFACE ( 'NONE', #5351, 2.500000000000002220 ) ;
#6620 = CARTESIAN_POINT ( 'NONE',  ( 3.796719365261179480, -2.062499999999996003, -1.574265350336458313 ) ) ;
#6621 = DIRECTION ( 'NONE',  ( -1.287488025362404182E-15, -1.000000000000000000, 0.000000000000000000 ) ) ;
#6622 = CARTESIAN_POINT ( 'NONE',  ( 1.603389813606017178, 11.99999970914575798, 0.01788390626213483964 ) ) ;
#6623 = EDGE_CURVE ( 'NONE', #12145, #6920, #1898, .T. ) ;
#6624 = EDGE_CURVE ( 'NONE', #12412, #8931, #9805, .T. ) ;
#6625 = DIRECTION ( 'NONE',  ( -1.000000000000000000, 0.000000000000000000, 0.000000000000000000 ) ) ;
#6626 = CARTESIAN_POINT ( 'NONE',  ( 3.016622086615760256, -0.8749999999999454880, 3.018230387793254810 ) ) ;
#6627 = CARTESIAN_POINT ( 'NONE',  ( -52.77438362644100067, 99.17411849586700612, -79.59847958357700293 ) ) ;
#6628 = CARTESIAN_POINT ( 'NONE',  ( 21.98164641901421135, -12.00000029085423670, -11.73358795631401463 ) ) ;
#6629 = VERTEX_POINT ( 'NONE', #6393 ) ;
#6630 = CARTESIAN_POINT ( 'NONE',  ( -5.196152422706630247, 0.1227504548087275521, -7.569115911492098221E-16 ) ) ;
#6631 = VERTEX_POINT ( 'NONE', #237 ) ;
#6632 = ORIENTED_EDGE ( 'NONE', *, *, #7341, .F. ) ;
#6633 = ORIENTED_EDGE ( 'NONE', *, *, #9615, .F. ) ;
#6634 = PLANE ( 'NONE',  #1778 ) ;
#6635 = CIRCLE ( 'NONE', #1159, 2.320576762250993852 ) ;
#6636 = CARTESIAN_POINT ( 'NONE',  ( 1.553520276525307997, -5.413125000000014175, 2.903814772855817239 ) ) ;
#6637 = EDGE_CURVE ( 'NONE', #8592, #4923, #13783, .T. ) ;
#6638 = AXIS2_PLACEMENT_3D ( 'NONE', #4426, #11330, #13816 ) ;
#6639 = PLANE ( 'NONE',  #8827 ) ;
#6640 = DIRECTION ( 'NONE',  ( 0.000000000000000000, 1.000000000000000000, 0.000000000000000000 ) ) ;
#6641 = DIRECTION ( 'NONE',  ( 0.000000000000000000, 0.000000000000000000, -1.000000000000000000 ) ) ;
#6642 = DIRECTION ( 'NONE',  ( -1.000000000000000000, 0.000000000000000000, 0.000000000000000000 ) ) ;
#6643 = CARTESIAN_POINT ( 'NONE',  ( -3.099447957106487461, -0.4995676945082667686, 2.829882024851861466 ) ) ;
#6644 = FACE_OUTER_BOUND ( 'NONE', #7837, .T. ) ;
#6645 = DIRECTION ( 'NONE',  ( 0.000000000000000000, -0.000000000000000000, -1.000000000000000000 ) ) ;
#6646 = ORIENTED_EDGE ( 'NONE', *, *, #14344, .F. ) ;
#6647 = AXIS2_PLACEMENT_3D ( 'NONE', #13763, #794, #8946 ) ;
#6648 = DIRECTION ( 'NONE',  ( 1.000000000000000000, 0.000000000000000000, 0.000000000000000000 ) ) ;
#6649 = ORIENTED_EDGE ( 'NONE', *, *, #346, .T. ) ;
#6650 = CIRCLE ( 'NONE', #2665, 1.785937500000001066 ) ;
#6651 = CARTESIAN_POINT ( 'NONE',  ( -52.77438362644100067, 103.4241184958670061, -145.4984795835769944 ) ) ;
#6652 = ORIENTED_EDGE ( 'NONE', *, *, #8404, .F. ) ;
#6653 = CARTESIAN_POINT ( 'NONE',  ( -3.582436959730881831, -2.421875000000131450, -1.916069189016956331 ) ) ;
#6654 = ORIENTED_EDGE ( 'NONE', *, *, #8010, .F. ) ;
#6655 = CYLINDRICAL_SURFACE ( 'NONE', #6489, 1.500000000000001332 ) ;
#6656 = VECTOR ( 'NONE', #14812, 1000.000000000000000 ) ;
#6657 = DIRECTION ( 'NONE',  ( 0.000000000000000000, 4.336808689942017736E-16, -1.000000000000000000 ) ) ;
#6658 = DIRECTION ( 'NONE',  ( 0.000000000000000000, 1.000000000000000000, 0.000000000000000000 ) ) ;
#6659 = CARTESIAN_POINT ( 'NONE',  ( -88.81638362644100937, 97.99516924618178848, -147.9984795835769944 ) ) ;
#6660 = DIRECTION ( 'NONE',  ( 0.000000000000000000, -0.000000000000000000, 1.000000000000000000 ) ) ;
#6661 = CARTESIAN_POINT ( 'NONE',  ( -55.47438362644099641, 99.17411849586700612, -145.4984795835769944 ) ) ;
#6662 = DIRECTION ( 'NONE',  ( 0.000000000000000000, 0.000000000000000000, -1.000000000000000000 ) ) ;
#6663 = VERTEX_POINT ( 'NONE', #13366 ) ;
#6664 = AXIS2_PLACEMENT_3D ( 'NONE', #13818, #12584, #3187 ) ;
#6665 = CARTESIAN_POINT ( 'NONE',  ( -0.2824495906440828152, 2.041549731959705837E-17, 21.57312693144813665 ) ) ;
#6666 = CARTESIAN_POINT ( 'NONE',  ( 0.3615547238501363170, -2.350625000000046150, 3.680709139401400432 ) ) ;
#6667 = ORIENTED_EDGE ( 'NONE', *, *, #4284, .T. ) ;
#6668 = ADVANCED_FACE ( 'NONE', ( #14429 ), #478, .T. ) ;
#6669 = DIRECTION ( 'NONE',  ( -0.000000000000000000, -0.000000000000000000, 1.000000000000000000 ) ) ;
#6670 = CARTESIAN_POINT ( 'NONE',  ( -54.81638362644100226, 97.99516924618178848, -147.9984795835769944 ) ) ;
#6671 = DIRECTION ( 'NONE',  ( -2.551930889570658776E-15, 1.000000000000000000, 0.000000000000000000 ) ) ;
#6672 = CIRCLE ( 'NONE', #15313, 2.000000000000001776 ) ;
#6673 = CARTESIAN_POINT ( 'NONE',  ( 22.58164641901421632, 11.99999970914576330, -11.73358795631400397 ) ) ;
#6674 = CARTESIAN_POINT ( 'NONE',  ( 22.58164641901421632, 3.729316161559856013, -0.3335879563140091153 ) ) ;
#6675 = CARTESIAN_POINT ( 'NONE',  ( -89.27438362644100778, 99.17411849586700612, -145.2984795835770058 ) ) ;
#6676 = VERTEX_POINT ( 'NONE', #3816 ) ;
#6677 = DIRECTION ( 'NONE',  ( -1.000000000000000000, 0.000000000000000000, 0.000000000000000000 ) ) ;
#6678 = EDGE_CURVE ( 'NONE', #6676, #12263, #11973, .T. ) ;
#6679 = ORIENTED_EDGE ( 'NONE', *, *, #2693, .T. ) ;
#6680 = ORIENTED_EDGE ( 'NONE', *, *, #7709, .T. ) ;
#6681 = ORIENTED_EDGE ( 'NONE', *, *, #4515, .T. ) ;
#6682 = VERTEX_POINT ( 'NONE', #5213 ) ;
#6683 = ORIENTED_EDGE ( 'NONE', *, *, #5578, .F. ) ;
#6684 = VECTOR ( 'NONE', #6879, 1000.000000000000000 ) ;
#6685 = CARTESIAN_POINT ( 'NONE',  ( -3.459955264279602094, -6.467963562372781361, -0.6891510056894314395 ) ) ;
#6686 = CARTESIAN_POINT ( 'NONE',  ( 2.697785604507370483, -1.459999999999946008, 2.699193867783821865 ) ) ;
#6687 = CARTESIAN_POINT ( 'NONE',  ( 1.186295216973591859, -2.203125000000055067, -3.915803815994934656 ) ) ;
#6688 = CARTESIAN_POINT ( 'NONE',  ( -16.74999999999999289, -0.3152037684892574076, 22.74589050208021490 ) ) ;
#6689 = CARTESIAN_POINT ( 'NONE',  ( 1.581646419014213878, 11.39999970914575655, 0.2664120436859911956 ) ) ;
#6690 = EDGE_CURVE ( 'NONE', #12176, #12493, #406, .T. ) ;
#6691 = FACE_OUTER_BOUND ( 'NONE', #11264, .T. ) ;
#6692 = CARTESIAN_POINT ( 'NONE',  ( -2.727692609523614475, -0.6406250000000671685, 3.321895092029963248 ) ) ;
#6693 = PLANE ( 'NONE',  #6590 ) ;
#6694 = DIRECTION ( 'NONE',  ( 0.000000000000000000, 0.000000000000000000, 1.000000000000000000 ) ) ;
#6695 = CARTESIAN_POINT ( 'NONE',  ( 16.75000000000000000, -0.3156864504677172611, 22.74361999681791602 ) ) ;
#6696 = EDGE_LOOP ( 'NONE', ( #2246, #2871, #3196, #6943, #9726 ) ) ;
#6697 = CARTESIAN_POINT ( 'NONE',  ( -69.77438362644001302, 94.57411849586699759, -89.99847958357699440 ) ) ;
#6698 = ADVANCED_FACE ( 'NONE', ( #3965 ), #8693, .F. ) ;
#6699 = ORIENTED_EDGE ( 'NONE', *, *, #11897, .T. ) ;
#6700 = ORIENTED_EDGE ( 'NONE', *, *, #13303, .F. ) ;
#6701 = EDGE_LOOP ( 'NONE', ( #7140, #9743, #1734 ) ) ;
#6702 = UNCERTAINTY_MEASURE_WITH_UNIT (LENGTH_MEASURE( 1.000000000000000082E-05 ), #6237, 'distance_accuracy_value', 'NONE');
#6703 = EDGE_CURVE ( 'NONE', #8453, #5033, #1488, .T. ) ;
#6704 = DIRECTION ( 'NONE',  ( 1.000000000000000000, 0.000000000000000000, 0.000000000000000000 ) ) ;
#6705 = ADVANCED_FACE ( 'NONE', ( #14355 ), #7470, .T. ) ;
#6706 = CARTESIAN_POINT ( 'NONE',  ( 2.417253850352953481, -4.460000000000003517, 2.418486108946755309 ) ) ;
#6707 = LINE ( 'NONE', #15202, #14774 ) ;
#6708 = CARTESIAN_POINT ( 'NONE',  ( -59.02799568714584666, 110.1741184958670061, -15.85886927678779834 ) ) ;
#6709 = FACE_OUTER_BOUND ( 'NONE', #15293, .T. ) ;
#6710 = EDGE_CURVE ( 'NONE', #3939, #3973, #7180, .T. ) ;
#6711 = DIRECTION ( 'NONE',  ( 0.000000000000000000, -0.000000000000000000, 1.000000000000000000 ) ) ;
#6712 = CARTESIAN_POINT ( 'NONE',  ( -72.41519636941028182, 75.17411849586697770, -44.45439862457464386 ) ) ;
#6713 = CYLINDRICAL_SURFACE ( 'NONE', #2838, 3.499999999999999556 ) ;
#6714 = CARTESIAN_POINT ( 'NONE',  ( 2.991299100910195019, -4.663125000000096776, -1.600316903339956243 ) ) ;
#6715 = ORIENTED_EDGE ( 'NONE', *, *, #8593, .F. ) ;
#6716 = CARTESIAN_POINT ( 'NONE',  ( 14.25000000000000000, -0.2038245569916330158, 23.22168783648699986 ) ) ;
#6717 = EDGE_CURVE ( 'NONE', #7102, #12263, #13052, .T. ) ;
#6718 = VERTEX_POINT ( 'NONE', #11027 ) ;
#6719 = EDGE_LOOP ( 'NONE', ( #15030, #5223, #10866, #15046 ) ) ;
#6720 = CARTESIAN_POINT ( 'NONE',  ( -4.125408418587476866, -0.5468750000000269784, 1.250226324283678192 ) ) ;
#6721 = EDGE_LOOP ( 'NONE', ( #4171, #10728, #4865, #13197 ) ) ;
#6722 = CARTESIAN_POINT ( 'NONE',  ( 2.518194796243166333, -3.139838562372984310, -3.066784450280832797 ) ) ;
#6723 = DIRECTION ( 'NONE',  ( -0.08715574274766167695, 0.000000000000000000, 0.9961946980917453232 ) ) ;
#6724 = DIRECTION ( 'NONE',  ( 0.000000000000000000, 0.000000000000000000, 1.000000000000000000 ) ) ;
#6725 = CARTESIAN_POINT ( 'NONE',  ( -69.77438362644001302, 82.17411849586700612, -43.99847958362880007 ) ) ;
#6726 = CARTESIAN_POINT ( 'NONE',  ( 15.50000000000000000, -0.4000000000000000222, 22.50000000000000000 ) ) ;
#6727 = CYLINDRICAL_SURFACE ( 'NONE', #12549, 0.6000000000000000888 ) ;
#6728 = CARTESIAN_POINT ( 'NONE',  ( -68.34858040079876673, 98.11273180361364155, -94.49612629051017620 ) ) ;
#6729 = DIRECTION ( 'NONE',  ( 0.000000000000000000, 1.000000000000000000, 0.000000000000000000 ) ) ;
#6730 = AXIS2_PLACEMENT_3D ( 'NONE', #6562, #14903, #647 ) ;
#6731 = DIRECTION ( 'NONE',  ( 0.000000000000000000, 0.000000000000000000, 1.000000000000000000 ) ) ;
#6732 = VERTEX_POINT ( 'NONE', #1641 ) ;
#6733 = VECTOR ( 'NONE', #5121, 1000.000000000000000 ) ;
#6734 = CARTESIAN_POINT ( 'NONE',  ( -3.080079348812820861, -0.1943750000000852018, 2.526399673485165032 ) ) ;
#6735 = ORIENTED_EDGE ( 'NONE', *, *, #10376, .F. ) ;
#6736 = CARTESIAN_POINT ( 'NONE',  ( -3.579091221414520518, -2.038125000000108322, -1.084269867492441586 ) ) ;
#6737 = DIRECTION ( 'NONE',  ( 0.000000000000000000, 0.000000000000000000, 1.000000000000000000 ) ) ;
#6738 = VECTOR ( 'NONE', #8791, 1000.000000000000000 ) ;
#6739 = DIRECTION ( 'NONE',  ( 0.000000000000000000, -0.000000000000000000, 1.000000000000000000 ) ) ;
#6740 = CARTESIAN_POINT ( 'NONE',  ( 3.992217303742939816, -0.4995676945082484499, -0.08329250675602982434 ) ) ;
#6741 = DIRECTION ( 'NONE',  ( 0.000000000000000000, 0.000000000000000000, 1.000000000000000000 ) ) ;
#6742 = EDGE_CURVE ( 'NONE', #1927, #14968, #4637, .T. ) ;
#6743 = CARTESIAN_POINT ( 'NONE',  ( 17.04394838817069413, 11.39999970914576011, 0.2824263826447109826 ) ) ;
#6744 = ORIENTED_EDGE ( 'NONE', *, *, #5639, .F. ) ;
#6745 = CARTESIAN_POINT ( 'NONE',  ( -13.41835358098578723, -11.40000029085424238, 0.2664120436859911956 ) ) ;
#6746 = ORIENTED_EDGE ( 'NONE', *, *, #2672, .T. ) ;
#6747 = CIRCLE ( 'NONE', #13688, 8.000000000000007105 ) ;
#6748 = ORIENTED_EDGE ( 'NONE', *, *, #10523, .T. ) ;
#6749 = ORIENTED_EDGE ( 'NONE', *, *, #518, .T. ) ;
#6750 = EDGE_LOOP ( 'NONE', ( #8884, #14380, #9347, #11967 ) ) ;
#6751 = ORIENTED_EDGE ( 'NONE', *, *, #7519, .T. ) ;
#6752 = CIRCLE ( 'NONE', #12934, 8.124999999999992895 ) ;
#6753 = CARTESIAN_POINT ( 'NONE',  ( -2.574205329084022331, -5.624213562373249431, 2.572875433237910681 ) ) ;
#6754 = VECTOR ( 'NONE', #3348, 1000.000000000000114 ) ;
#6755 = CARTESIAN_POINT ( 'NONE',  ( -3.693744850241972077, -1.131875000000025722, 1.119430425315776523 ) ) ;
#6756 = FILL_AREA_STYLE ('',( #1939 ) ) ;
#6757 = CARTESIAN_POINT ( 'NONE',  ( -2.852666340614860463, -2.624999999999946265, 2.854740429567705018 ) ) ;
#6758 = LINE ( 'NONE', #2087, #8250 ) ;
#6759 = ADVANCED_FACE ( 'NONE', ( #7316 ), #308, .T. ) ;
#6760 = LINE ( 'NONE', #3030, #3151 ) ;
#6761 = AXIS2_PLACEMENT_3D ( 'NONE', #1396, #12249, #4897 ) ;
#6762 = CARTESIAN_POINT ( 'NONE',  ( 3.331139167509270749, 2.239389106484354297, 3.230297714791237507 ) ) ;
#6763 = CARTESIAN_POINT ( 'NONE',  ( 3.935370341889717682, -0.9375000000000351941, 1.628420556316443557 ) ) ;
#6764 = DIRECTION ( 'NONE',  ( 1.000000000000000000, 0.000000000000000000, 0.000000000000000000 ) ) ;
#6765 = DIRECTION ( 'NONE',  ( 0.000000000000000000, 0.000000000000000000, 1.000000000000000000 ) ) ;
#6766 = ADVANCED_FACE ( 'NONE', ( #399 ), #13881, .T. ) ;
#6767 = CARTESIAN_POINT ( 'NONE',  ( -16.54686605390241994, -0.2715358723599897717, -21.66103272505201360 ) ) ;
#6768 = VERTEX_POINT ( 'NONE', #12421 ) ;
#6769 = PLANE ( 'NONE',  #13706 ) ;
#6770 = VECTOR ( 'NONE', #440, 1000.000000000000000 ) ;
#6771 = ORIENTED_EDGE ( 'NONE', *, *, #8490, .T. ) ;
#6772 = ORIENTED_EDGE ( 'NONE', *, *, #6884, .F. ) ;
#6773 = ORIENTED_EDGE ( 'NONE', *, *, #5748, .F. ) ;
#6774 = AXIS2_PLACEMENT_3D ( 'NONE', #13294, #12193, #11032 ) ;
#6775 = DIRECTION ( 'NONE',  ( 0.000000000000000000, 0.000000000000000000, 1.000000000000000000 ) ) ;
#6776 = CARTESIAN_POINT ( 'NONE',  ( -3.468991550463924156, -4.085000000000062137, -0.0008868951686453910126 ) ) ;
#6777 = CARTESIAN_POINT ( 'NONE',  ( -69.77438362644001302, 82.17411849586700612, -182.1969643934119745 ) ) ;
#6778 = DIRECTION ( 'NONE',  ( 0.000000000000000000, 1.000000000000000000, 0.000000000000000000 ) ) ;
#6779 = EDGE_CURVE ( 'NONE', #14576, #12703, #5896, .T. ) ;
#6780 = AXIS2_PLACEMENT_3D ( 'NONE', #14819, #3038, #705 ) ;
#6781 = CARTESIAN_POINT ( 'NONE',  ( -86.77438362644001302, 65.17411849586700612, -145.4984795835769660 ) ) ;
#6782 = CARTESIAN_POINT ( 'NONE',  ( 15.50000000000000000, -1.037157890325000054, -22.50000000000000000 ) ) ;
#6783 = CARTESIAN_POINT ( 'NONE',  ( -54.81638362644000040, 63.99516924618178848, -147.9984795835769944 ) ) ;
#6784 = CARTESIAN_POINT ( 'NONE',  ( 22.58164641901421632, 3.729316161559856013, -0.3335879563140091153 ) ) ;
#6785 = EDGE_CURVE ( 'NONE', #12175, #2233, #1922, .T. ) ;
#6786 = VECTOR ( 'NONE', #7152, 1000.000000000000000 ) ;
#6787 = ORIENTED_EDGE ( 'NONE', *, *, #9420, .F. ) ;
#6788 = CARTESIAN_POINT ( 'NONE',  ( -60.43728955831366534, 68.38713492810558137, -83.44847958357698303 ) ) ;
#6789 = ORIENTED_EDGE ( 'NONE', *, *, #3741, .T. ) ;
#6790 = ORIENTED_EDGE ( 'NONE', *, *, #13519, .F. ) ;
#6791 = CARTESIAN_POINT ( 'NONE',  ( -66.41143315690761995, 66.60412428008086749, -81.84847958357697451 ) ) ;
#6792 = AXIS2_PLACEMENT_3D ( 'NONE', #4835, #15287, #2187 ) ;
#6793 = ORIENTED_EDGE ( 'NONE', *, *, #2848, .T. ) ;
#6794 = VECTOR ( 'NONE', #8681, 1000.000000000000000 ) ;
#6795 = ADVANCED_FACE ( 'NONE', ( #4267 ), #2009, .F. ) ;
#6796 = CARTESIAN_POINT ( 'NONE',  ( -2.948053448091068507, -1.625000000000079936, 2.946489148067756858 ) ) ;
#6797 = EDGE_LOOP ( 'NONE', ( #12516, #6523 ) ) ;
#6798 = CARTESIAN_POINT ( 'NONE',  ( -3.971205795094620683, -2.530463562372954112, 0.7888322869661125170 ) ) ;
#6799 = DIRECTION ( 'NONE',  ( 0.000000000000000000, 0.5000000000000199840, 0.8660254037844271613 ) ) ;
#6800 = EDGE_CURVE ( 'NONE', #11016, #12055, #3894, .T. ) ;
#6801 = FACE_OUTER_BOUND ( 'NONE', #6195, .T. ) ;
#6802 = LINE ( 'NONE', #10265, #12226 ) ;
#6803 = VECTOR ( 'NONE', #5053, 1000.000000000000000 ) ;
#6804 = CONICAL_SURFACE ( 'NONE', #2830, 3.749999999999996447, 0.7853981633974476129 ) ;
#6805 = EDGE_CURVE ( 'NONE', #14347, #7919, #4381, .T. ) ;
#6806 = DIRECTION ( 'NONE',  ( 0.000000000000000000, 0.000000000000000000, 1.000000000000000000 ) ) ;
#6807 = ADVANCED_FACE ( 'NONE', ( #6839 ), #1866, .F. ) ;
#6808 = CARTESIAN_POINT ( 'NONE',  ( -68.62457557633291572, 98.13530264660337821, -94.57468145058379605 ) ) ;
#6809 = LINE ( 'NONE', #9181, #49 ) ;
#6810 = VERTEX_POINT ( 'NONE', #11257 ) ;
#6811 = DIRECTION ( 'NONE',  ( 0.000000000000000000, 0.000000000000000000, -1.000000000000000000 ) ) ;
#6812 = CARTESIAN_POINT ( 'NONE',  ( 3.291891004236185747, -4.921874999999971578, 1.757997479805845975 ) ) ;
#6813 = EDGE_LOOP ( 'NONE', ( #1627, #6217 ) ) ;
#6814 = AXIS2_PLACEMENT_3D ( 'NONE', #14359, #7318, #8621 ) ;
#6815 = VECTOR ( 'NONE', #7202, 1000.000000000000114 ) ;
#6816 = CARTESIAN_POINT ( 'NONE',  ( 0.7342756466162075890, -1.803750000000060361, -3.698544502508174681 ) ) ;
#6817 = LINE ( 'NONE', #2068, #14874 ) ;
#6818 = FACE_OUTER_BOUND ( 'NONE', #7227, .T. ) ;
#6819 = LINE ( 'NONE', #11539, #4309 ) ;
#6820 = CARTESIAN_POINT ( 'NONE',  ( 3.931003132613788420, -0.4995676945082495601, 0.5405018855187671001 ) ) ;
#6821 = CARTESIAN_POINT ( 'NONE',  ( 3.530157234965975555, -5.226201182446649440, -2.246195850846843811E-13 ) ) ;
#6822 = DIRECTION ( 'NONE',  ( 0.000000000000000000, -0.000000000000000000, 1.000000000000000000 ) ) ;
#6823 = FACE_OUTER_BOUND ( 'NONE', #6384, .T. ) ;
#6824 = ORIENTED_EDGE ( 'NONE', *, *, #6578, .T. ) ;
#6825 = AXIS2_PLACEMENT_3D ( 'NONE', #8998, #3252, #2092 ) ;
#6826 = CARTESIAN_POINT ( 'NONE',  ( -12.81835358098578759, -12.40000029085423883, -9.367156043074160721 ) ) ;
#6827 = ORIENTED_EDGE ( 'NONE', *, *, #576, .T. ) ;
#6828 = ORIENTED_EDGE ( 'NONE', *, *, #125, .F. ) ;
#6829 = CARTESIAN_POINT ( 'NONE',  ( -3.069066067673342779, -4.006874999999906706, -1.638984897852512113 ) ) ;
#6830 = VERTEX_POINT ( 'NONE', #5448 ) ;
#6831 = VERTEX_POINT ( 'NONE', #5523 ) ;
#6832 = ORIENTED_EDGE ( 'NONE', *, *, #2864, .F. ) ;
#6833 = CARTESIAN_POINT ( 'NONE',  ( -3.050941831956043515, -5.405463562373032715, -2.036948827022558195 ) ) ;
#6834 = PRESENTATION_LAYER_ASSIGNMENT (  '', '', ( #8805 ) ) ;
#6835 = CARTESIAN_POINT ( 'NONE',  ( -3.080079348812917228, -0.1943750000000852018, 2.526399673485165032 ) ) ;
#6836 = CARTESIAN_POINT ( 'NONE',  ( 0.7355390728087518593, -5.399066645772633066, 3.225404868253181956 ) ) ;
#6837 = AXIS2_PLACEMENT_3D ( 'NONE', #11688, #3467, #3631 ) ;
#6838 = CARTESIAN_POINT ( 'NONE',  ( 3.434081308463064364, -1.906250000000116795, 2.295896066549416581 ) ) ;
#6839 = FACE_OUTER_BOUND ( 'NONE', #10740, .T. ) ;
#6840 = CARTESIAN_POINT ( 'NONE',  ( -48.52438362643999881, 65.17411849586700612, -149.9984795835770228 ) ) ;
#6841 = LINE ( 'NONE', #10313, #1120 ) ;
#6842 = DIRECTION ( 'NONE',  ( 0.000000000000000000, 0.000000000000000000, 1.000000000000000000 ) ) ;
#6843 = CARTESIAN_POINT ( 'NONE',  ( -64.53565528768383786, 67.29799558322736175, -81.84847958357697451 ) ) ;
#6844 = ORIENTED_EDGE ( 'NONE', *, *, #14265, .F. ) ;
#6845 = DIRECTION ( 'NONE',  ( 0.000000000000000000, 1.000000000000000000, 0.000000000000000000 ) ) ;
#6846 = EDGE_LOOP ( 'NONE', ( #5943, #1934, #2831, #3093 ) ) ;
#6847 = AXIS2_PLACEMENT_3D ( 'NONE', #4460, #6724, #8958 ) ;
#6848 = ORIENTED_EDGE ( 'NONE', *, *, #14135, .T. ) ;
#6849 = ORIENTED_EDGE ( 'NONE', *, *, #9061, .T. ) ;
#6850 = VECTOR ( 'NONE', #5226, 1000.000000000000000 ) ;
#6851 = EDGE_CURVE ( 'NONE', #2365, #14049, #6146, .T. ) ;
#6852 = CARTESIAN_POINT ( 'NONE',  ( -84.02438362643999881, 65.17411849586700612, -152.4984795835769944 ) ) ;
#6853 = EDGE_CURVE ( 'NONE', #3706, #8985, #12580, .T. ) ;
#6854 = CYLINDRICAL_SURFACE ( 'NONE', #4877, 10.50000000000000178 ) ;
#6855 = AXIS2_PLACEMENT_3D ( 'NONE', #6321, #10013, #3035 ) ;
#6856 = CARTESIAN_POINT ( 'NONE',  ( -86.77438362643999881, 65.17411849586700612, -79.59847958357700293 ) ) ;
#6857 = CARTESIAN_POINT ( 'NONE',  ( 0.4577183132938494881, 2.374744442185180215, -4.499999999999999112 ) ) ;
#6858 = LINE ( 'NONE', #11500, #4627 ) ;
#6859 = VECTOR ( 'NONE', #4216, 1000.000000000000000 ) ;
#6860 = CARTESIAN_POINT ( 'NONE',  ( -84.73238362644100619, 99.17411849586700612, -147.9984795835769944 ) ) ;
#6861 = CARTESIAN_POINT ( 'NONE',  ( -35.58670980944424400, 5.000000000000001776, 97.50956111919106206 ) ) ;
#6862 = CARTESIAN_POINT ( 'NONE',  ( -54.81638362644100226, 100.3530677455522238, -150.4984795835770228 ) ) ;
#6863 = ORIENTED_EDGE ( 'NONE', *, *, #10184, .T. ) ;
#6864 = LINE ( 'NONE', #3593, #8606 ) ;
#6865 = ORIENTED_EDGE ( 'NONE', *, *, #9121, .T. ) ;
#6866 = VERTEX_POINT ( 'NONE', #14878 ) ;
#6867 = FACE_OUTER_BOUND ( 'NONE', #5049, .T. ) ;
#6868 = VECTOR ( 'NONE', #13004, 1000.000000000000114 ) ;
#6869 = EDGE_CURVE ( 'NONE', #6026, #2695, #13660, .T. ) ;
#6870 = EDGE_LOOP ( 'NONE', ( #7104, #4377 ) ) ;
#6871 = CARTESIAN_POINT ( 'NONE',  ( -0.8118119174735605181, -1.718749999999964917, 4.075604227461077755 ) ) ;
#6872 = ORIENTED_EDGE ( 'NONE', *, *, #11139, .T. ) ;
#6873 = CARTESIAN_POINT ( 'NONE',  ( 2.540175370683049216, -2.858588562373145070, 3.096875823539658068 ) ) ;
#6874 = CARTESIAN_POINT ( 'NONE',  ( -69.77438362644001302, 82.17411849586700612, -93.49847958357699440 ) ) ;
#6875 = CARTESIAN_POINT ( 'NONE',  ( -11.54813546431719473, 5.000000000000000000, 11.54813546431703308 ) ) ;
#6876 = AXIS2_PLACEMENT_3D ( 'NONE', #5944, #5705, #4525 ) ;
#6877 = AXIS2_PLACEMENT_3D ( 'NONE', #1694, #7606, #12329 ) ;
#6878 = EDGE_CURVE ( 'NONE', #3986, #14025, #8601, .T. ) ;
#6879 = DIRECTION ( 'NONE',  ( -1.000000000000000000, 0.000000000000000000, 0.000000000000000000 ) ) ;
#6880 = ORIENTED_EDGE ( 'NONE', *, *, #12556, .T. ) ;
#6881 = EDGE_CURVE ( 'NONE', #6165, #7621, #7698, .T. ) ;
#6882 = FACE_OUTER_BOUND ( 'NONE', #2936, .T. ) ;
#6883 = DIRECTION ( 'NONE',  ( -1.000000000000000000, -1.747085166004344019E-15, 0.000000000000000000 ) ) ;
#6884 = EDGE_CURVE ( 'NONE', #11036, #4583, #6760, .T. ) ;
#6885 = EDGE_LOOP ( 'NONE', ( #10387, #12155, #15196, #11430 ) ) ;
#6886 = FACE_OUTER_BOUND ( 'NONE', #2272, .T. ) ;
#6887 = CARTESIAN_POINT ( 'NONE',  ( -3.385327830538905847, -5.437500000000312639, -1.400787550305463203 ) ) ;
#6888 = ORIENTED_EDGE ( 'NONE', *, *, #975, .T. ) ;
#6889 = ADVANCED_FACE ( 'NONE', ( #4351 ), #3389, .F. ) ;
#6890 = AXIS2_PLACEMENT_3D ( 'NONE', #6931, #3204, #5627 ) ;
#6891 = ADVANCED_FACE ( 'NONE', ( #7773 ), #661, .T. ) ;
#6892 = CARTESIAN_POINT ( 'NONE',  ( 0.3615547238501363725, -2.350625000000046150, 3.680709139401309837 ) ) ;
#6893 = FACE_OUTER_BOUND ( 'NONE', #13388, .T. ) ;
#6894 = DIRECTION ( 'NONE',  ( 1.000000000000000000, -0.000000000000000000, 0.000000000000000000 ) ) ;
#6895 = EDGE_CURVE ( 'NONE', #14169, #11388, #13593, .T. ) ;
#6896 = DIRECTION ( 'NONE',  ( 0.000000000000000000, 0.000000000000000000, 1.000000000000000000 ) ) ;
#6897 =( NAMED_UNIT ( * ) SI_UNIT ( $, .STERADIAN. ) SOLID_ANGLE_UNIT ( ) );
#6898 = DIRECTION ( 'NONE',  ( 0.000000000000000000, 4.336808689942017736E-16, -1.000000000000000000 ) ) ;
#6899 = DIRECTION ( 'NONE',  ( -0.8660254037844485886, 0.000000000000000000, -0.4999999999999827360 ) ) ;
#6900 = VECTOR ( 'NONE', #8064, 1000.000000000000000 ) ;
#6901 = ORIENTED_EDGE ( 'NONE', *, *, #3741, .F. ) ;
#6902 = DIRECTION ( 'NONE',  ( 0.000000000000000000, 0.5000000000000189848, 0.8660254037844277164 ) ) ;
#6903 = EDGE_CURVE ( 'NONE', #9613, #8453, #1785, .T. ) ;
#6904 = VERTEX_POINT ( 'NONE', #3645 ) ;
#6905 = EDGE_LOOP ( 'NONE', ( #11268, #13127, #10891, #9167 ) ) ;
#6906 = CARTESIAN_POINT ( 'NONE',  ( -1.287538504857992594, -4.897500000000167830, -3.105113058795574865 ) ) ;
#6907 = VERTEX_POINT ( 'NONE', #8296 ) ;
#6908 = ORIENTED_EDGE ( 'NONE', *, *, #4221, .F. ) ;
#6909 = ORIENTED_EDGE ( 'NONE', *, *, #2013, .T. ) ;
#6910 = CARTESIAN_POINT ( 'NONE',  ( -3.116388545455692771, -6.421088562373019393, -1.666773181135335902 ) ) ;
#6911 = CARTESIAN_POINT ( 'NONE',  ( -2.746234728672232173, -0.9599999999999920819, -2.744228674164098436 ) ) ;
#6912 = AXIS2_PLACEMENT_3D ( 'NONE', #13400, #7589, #9890 ) ;
#6913 = CARTESIAN_POINT ( 'NONE',  ( 1.869272562217232592, -3.171875000000011990, -3.494952631674145938 ) ) ;
#6914 = CARTESIAN_POINT ( 'NONE',  ( -15.50000000000000000, -2.500000000000000000, 21.05662432702600029 ) ) ;
#6915 = CARTESIAN_POINT ( 'NONE',  ( -91.27438362643999881, 65.17411849586700612, -79.59847958357700293 ) ) ;
#6916 = CARTESIAN_POINT ( 'NONE',  ( 21.98164641901421135, 11.39999970914576366, -11.73358795631400397 ) ) ;
#6917 = CARTESIAN_POINT ( 'NONE',  ( 10.10406781373725771, 10.99999970914572600, 69.08979243323354069 ) ) ;
#6918 = DIRECTION ( 'NONE',  ( -0.000000000000000000, 0.000000000000000000, -1.000000000000000000 ) ) ;
#6919 = CARTESIAN_POINT ( 'NONE',  ( -14.25000000000000000, -2.500000000000000000, 23.22168783648699986 ) ) ;
#6920 = VERTEX_POINT ( 'NONE', #6915 ) ;
#6921 = LINE ( 'NONE', #3490, #4052 ) ;
#6922 = EDGE_LOOP ( 'NONE', ( #9759, #6939, #2896 ) ) ;
#6923 = AXIS2_PLACEMENT_3D ( 'NONE', #8654, #5105, #14386 ) ;
#6924 = EDGE_LOOP ( 'NONE', ( #14647, #6751, #13219, #1482, #4112 ) ) ;
#6925 = ORIENTED_EDGE ( 'NONE', *, *, #769, .F. ) ;
#6926 = FACE_OUTER_BOUND ( 'NONE', #10135, .T. ) ;
#6927 = CARTESIAN_POINT ( 'NONE',  ( 15.50000000000000000, -0.2038245569916610489, 21.05662432702600029 ) ) ;
#6928 = CARTESIAN_POINT ( 'NONE',  ( -66.51083064278975598, 75.17411849586699191, -44.70344037800771275 ) ) ;
#6929 = CARTESIAN_POINT ( 'NONE',  ( 2.192040893887766018, 1.873195365157829473, -4.499999999999998224 ) ) ;
#6930 = CARTESIAN_POINT ( 'NONE',  ( -55.47438362644000165, 65.17411849586700612, -145.2984795835770058 ) ) ;
#6931 = CARTESIAN_POINT ( 'NONE',  ( -86.77438362644100778, 99.17411849586700612, -147.9984795835769944 ) ) ;
#6932 = PLANE ( 'NONE',  #10240 ) ;
#6933 = DIRECTION ( 'NONE',  ( 1.000000000000000000, 0.000000000000000000, 0.000000000000000000 ) ) ;
#6934 = CARTESIAN_POINT ( 'NONE',  ( 16.75000000000000000, -2.500000000000000000, -21.77831216351300014 ) ) ;
#6935 = ORIENTED_EDGE ( 'NONE', *, *, #4127, .T. ) ;
#6936 = FACE_OUTER_BOUND ( 'NONE', #3397, .T. ) ;
#6937 = ADVANCED_FACE ( 'NONE', ( #10382, #2165 ), #9375, .F. ) ;
#6938 = ORIENTED_EDGE ( 'NONE', *, *, #3195, .F. ) ;
#6939 = ORIENTED_EDGE ( 'NONE', *, *, #9503, .T. ) ;
#6940 = CARTESIAN_POINT ( 'NONE',  ( -64.53565528768383786, 67.29799558322736175, -83.44847958357698303 ) ) ;
#6941 = ORIENTED_EDGE ( 'NONE', *, *, #4110, .F. ) ;
#6942 = CARTESIAN_POINT ( 'NONE',  ( -4.166404709851690313, -1.484374999999892752, -0.4114723880711238513 ) ) ;
#6943 = ORIENTED_EDGE ( 'NONE', *, *, #13413, .F. ) ;
#6944 = CARTESIAN_POINT ( 'NONE',  ( 1.188938652636758464, -2.202338562373083342, -3.915676949994142397 ) ) ;
#6945 = CARTESIAN_POINT ( 'NONE',  ( -77.94906324475290660, 70.01464610989972925, -83.44847958357698303 ) ) ;
#6946 = CARTESIAN_POINT ( 'NONE',  ( -15.50000000000000000, -2.500000000000000000, -21.05662432702600029 ) ) ;
#6947 = CARTESIAN_POINT ( 'NONE',  ( 4.353714886931038031, 2.288586792248405555, -1.459144614166440146 ) ) ;
#6948 = ADVANCED_FACE ( 'NONE', ( #14264 ), #5686, .F. ) ;
#6949 = DIRECTION ( 'NONE',  ( 0.000000000000000000, 0.000000000000000000, -1.000000000000000000 ) ) ;
#6950 = ORIENTED_EDGE ( 'NONE', *, *, #14443, .F. ) ;
#6951 = DIRECTION ( 'NONE',  ( 1.000000000000000000, 0.000000000000000000, 0.000000000000000000 ) ) ;
#6952 = ADVANCED_FACE ( 'NONE', ( #998 ), #11708, .F. ) ;
#6953 = DIRECTION ( 'NONE',  ( 0.9378889346118977066, 0.3469356515732558988, 0.000000000000000000 ) ) ;
#6954 = VERTEX_POINT ( 'NONE', #15263 ) ;
#6955 = FACE_OUTER_BOUND ( 'NONE', #12034, .T. ) ;
#6956 = CARTESIAN_POINT ( 'NONE',  ( 1.071213019063891991, -5.203124999999990230, -3.535999920922690443 ) ) ;
#6957 = ORIENTED_EDGE ( 'NONE', *, *, #8207, .F. ) ;
#6958 = CARTESIAN_POINT ( 'NONE',  ( -3.657957510581538507, -2.116249999999859632, 0.7266254446581354998 ) ) ;
#6959 = DIRECTION ( 'NONE',  ( 0.000000000000000000, 0.000000000000000000, 1.000000000000000000 ) ) ;
#6960 = ADVANCED_FACE ( 'NONE', ( #3482 ), #3563, .F. ) ;
#6961 = DIRECTION ( 'NONE',  ( 0.000000000000000000, 0.000000000000000000, 1.000000000000000000 ) ) ;
#6962 = CARTESIAN_POINT ( 'NONE',  ( 11.02010870769206541, -11.00000029085428110, 70.09311034953164210 ) ) ;
#6963 = DIRECTION ( 'NONE',  ( -0.000000000000000000, 1.000000000000000000, 4.336808689942017736E-16 ) ) ;
#6964 = CARTESIAN_POINT ( 'NONE',  ( -65.90140028023573393, 75.17411849586525818, -44.99847958359791278 ) ) ;
#6965 = EDGE_CURVE ( 'NONE', #11097, #557, #13041, .T. ) ;
#6966 = DIRECTION ( 'NONE',  ( 0.000000000000000000, 0.000000000000000000, -1.000000000000000000 ) ) ;
#6967 = CIRCLE ( 'NONE', #9430, 4.499999999999997335 ) ;
#6968 = EDGE_CURVE ( 'NONE', #897, #682, #14534, .T. ) ;
#6969 = ORIENTED_EDGE ( 'NONE', *, *, #5262, .T. ) ;
#6970 = LINE ( 'NONE', #6745, #2566 ) ;
#6971 = EDGE_LOOP ( 'NONE', ( #10389, #755, #11820 ) ) ;
#6972 = VERTEX_POINT ( 'NONE', #64 ) ;
#6973 = CARTESIAN_POINT ( 'NONE',  ( -2.874539946219752728, -4.178749999999989306, 1.919644203647528524 ) ) ;
#6974 = EDGE_LOOP ( 'NONE', ( #12746, #5946, #13392, #6305 ) ) ;
#6975 = ORIENTED_EDGE ( 'NONE', *, *, #8364, .T. ) ;
#6976 = EDGE_LOOP ( 'NONE', ( #4937, #3319, #5458, #5979 ) ) ;
#6977 = CIRCLE ( 'NONE', #14632, 0.5999999999999998668 ) ;
#6978 = CARTESIAN_POINT ( 'NONE',  ( 2.866736077644334912, -5.108588562372962549, -2.351425311670667817 ) ) ;
#6979 = EDGE_CURVE ( 'NONE', #5837, #13053, #8217, .T. ) ;
#6980 = CYLINDRICAL_SURFACE ( 'NONE', #3829, 4.000000000000000000 ) ;
#6981 = CIRCLE ( 'NONE', #1277, 4.249999999999996447 ) ;
#6982 = DIRECTION ( 'NONE',  ( -0.000000000000000000, 0.000000000000000000, -1.000000000000000000 ) ) ;
#6983 = CYLINDRICAL_SURFACE ( 'NONE', #3049, 10.50000000000000178 ) ;
#6984 = ADVANCED_FACE ( 'NONE', ( #10537 ), #5916, .T. ) ;
#6985 = PLANE ( 'NONE',  #5133 ) ;
#6986 = DIRECTION ( 'NONE',  ( 0.000000000000000000, 0.000000000000000000, -1.000000000000000000 ) ) ;
#6987 = FACE_OUTER_BOUND ( 'NONE', #3841, .T. ) ;
#6988 = LINE ( 'NONE', #15268, #9558 ) ;
#6989 = CARTESIAN_POINT ( 'NONE',  ( -3.199287326323787095, -5.038124999999881837, -0.9691876696830878934 ) ) ;
#6990 = ADVANCED_FACE ( 'NONE', ( #12958 ), #6985, .F. ) ;
#6991 = CARTESIAN_POINT ( 'NONE',  ( 68.41329019055577021, 0.000000000000000000, 137.5095611191910621 ) ) ;
#6992 = VECTOR ( 'NONE', #15142, 1000.000000000000000 ) ;
#6993 = EDGE_CURVE ( 'NONE', #5515, #9845, #15185, .T. ) ;
#6994 = ORIENTED_EDGE ( 'NONE', *, *, #2672, .F. ) ;
#6995 = CARTESIAN_POINT ( 'NONE',  ( -85.83938362643999653, 81.46011849586699327, -81.84847958357697451 ) ) ;
#6996 = ORIENTED_EDGE ( 'NONE', *, *, #7964, .F. ) ;
#6997 = AXIS2_PLACEMENT_3D ( 'NONE', #14199, #3659, #8232 ) ;
#6998 = VERTEX_POINT ( 'NONE', #13118 ) ;
#6999 = ORIENTED_EDGE ( 'NONE', *, *, #12106, .T. ) ;
#7000 = AXIS2_PLACEMENT_3D ( 'NONE', #666, #5419, #14853 ) ;
#7001 = CARTESIAN_POINT ( 'NONE',  ( -0.3378546177656944205, -4.319374999999974207, 3.421346328963575711 ) ) ;
#7002 = VECTOR ( 'NONE', #3584, 1000.000000000000000 ) ;
#7003 = CARTESIAN_POINT ( 'NONE',  ( 14.45366306705350112, -0.2717122460102528447, 21.66072723692567692 ) ) ;
#7004 = CARTESIAN_POINT ( 'NONE',  ( 22.33311828159035883, -3.654316742536411144, 0.2664120436859908625 ) ) ;
#7005 = CARTESIAN_POINT ( 'NONE',  ( -91.27438362643999881, 99.17411849586700612, -86.49847958357699440 ) ) ;
#7006 = LINE ( 'NONE', #10801, #13307 ) ;
#7007 = AXIS2_PLACEMENT_3D ( 'NONE', #816, #9114, #13928 ) ;
#7008 = LINE ( 'NONE', #12742, #2414 ) ;
#7009 = CARTESIAN_POINT ( 'NONE',  ( -52.77438362643999881, 62.81621999649657084, -147.9984795835769944 ) ) ;
#7010 = LINE ( 'NONE', #171, #3839 ) ;
#7011 = CARTESIAN_POINT ( 'NONE',  ( -80.52077156573417938, 0.000000000000000000, -79.59847958357700293 ) ) ;
#7012 = ORIENTED_EDGE ( 'NONE', *, *, #9522, .T. ) ;
#7013 = DIRECTION ( 'NONE',  ( 0.000000000000000000, -1.000000000000000000, 0.000000000000000000 ) ) ;
#7014 = ORIENTED_EDGE ( 'NONE', *, *, #7216, .T. ) ;
#7015 = ORIENTED_EDGE ( 'NONE', *, *, #10238, .F. ) ;
#7016 = DIRECTION ( 'NONE',  ( 0.000000000000000000, 0.000000000000000000, 1.000000000000000000 ) ) ;
#7017 = VERTEX_POINT ( 'NONE', #4811 ) ;
#7018 = CARTESIAN_POINT ( 'NONE',  ( -3.428831060970971567, 0.3906249999999135136, 2.812429823455744327 ) ) ;
#7019 = ORIENTED_EDGE ( 'NONE', *, *, #11344, .F. ) ;
#7020 = CIRCLE ( 'NONE', #12696, 4.000000000000000888 ) ;
#7021 = CARTESIAN_POINT ( 'NONE',  ( 1.891342852395442531, -2.827338562373011399, 3.535359886477475566 ) ) ;
#7022 = VECTOR ( 'NONE', #12110, 1000.000000000000000 ) ;
#7023 = CARTESIAN_POINT ( 'NONE',  ( -86.77438362644001302, 99.17411849586700612, -145.4984795835769660 ) ) ;
#7024 = DIRECTION ( 'NONE',  ( 0.000000000000000000, 0.000000000000000000, -1.000000000000000000 ) ) ;
#7025 = AXIS2_PLACEMENT_3D ( 'NONE', #6095, #9324, #3591 ) ;
#7026 = DIRECTION ( 'NONE',  ( 1.000000000000000000, 0.000000000000000000, 0.000000000000000000 ) ) ;
#7027 = CARTESIAN_POINT ( 'NONE',  ( -12.81835358098578403, 12.59999970914575940, -8.183940086454237317 ) ) ;
#7028 = ORIENTED_EDGE ( 'NONE', *, *, #9680, .T. ) ;
#7029 = DIRECTION ( 'NONE',  ( -0.8660254037844482555, 0.000000000000000000, 0.4999999999999831801 ) ) ;
#7030 = AXIS2_PLACEMENT_3D ( 'NONE', #14996, #5566, #2132 ) ;
#7031 = AXIS2_PLACEMENT_3D ( 'NONE', #5736, #5509, #8133 ) ;
#7032 = DIRECTION ( 'NONE',  ( 0.000000000000000000, 1.000000000000000000, 0.000000000000000000 ) ) ;
#7033 = PRODUCT_CONTEXT ( 'NONE', #2468, 'mechanical' ) ;
#7034 = EDGE_LOOP ( 'NONE', ( #8842, #8843, #14985, #12159 ) ) ;
#7035 = CIRCLE ( 'NONE', #335, 1.449999999999999956 ) ;
#7036 = SURFACE_STYLE_FILL_AREA ( #10903 ) ;
#7037 = CARTESIAN_POINT ( 'NONE',  ( 2.481497852716000097, -0.7256250000000298295, -3.025965195089417747 ) ) ;
#7038 = ORIENTED_EDGE ( 'NONE', *, *, #12766, .T. ) ;
#7039 = ADVANCED_FACE ( 'NONE', ( #7217 ), #4659, .F. ) ;
#7040 = CARTESIAN_POINT ( 'NONE',  ( 2.674095735623811088, -1.709999999999972209, -2.676057788957662886 ) ) ;
#7041 = CIRCLE ( 'NONE', #343, 17.00000000000000000 ) ;
#7042 = CARTESIAN_POINT ( 'NONE',  ( -52.77438362643999881, 67.53201699523744139, -147.9984795835769944 ) ) ;
#7043 = EDGE_CURVE ( 'NONE', #13047, #5763, #646, .T. ) ;
#7044 = VECTOR ( 'NONE', #683, 1000.000000000000000 ) ;
#7045 = CARTESIAN_POINT ( 'NONE',  ( -58.27438362644001302, 82.17411849586700612, -82.44847958357698303 ) ) ;
#7046 = DIRECTION ( 'NONE',  ( 0.000000000000000000, 0.000000000000000000, 1.000000000000000000 ) ) ;
#7047 = DIRECTION ( 'NONE',  ( 1.000000000000000000, 0.000000000000000000, 0.000000000000000000 ) ) ;
#7048 = CARTESIAN_POINT ( 'NONE',  ( 57.41329019055577021, 0.000000000000000000, 97.50956111919106206 ) ) ;
#7049 = CARTESIAN_POINT ( 'NONE',  ( -23.24999999999999289, -5.000000000000000000, 27.00000000000000000 ) ) ;
#7050 = DIRECTION ( 'NONE',  ( 0.000000000000000000, 0.000000000000000000, -1.000000000000000000 ) ) ;
#7051 = EDGE_LOOP ( 'NONE', ( #2077, #8305, #7481, #6938, #6828 ) ) ;
#7052 = DIRECTION ( 'NONE',  ( -0.000000000000000000, 1.000000000000000000, -0.000000000000000000 ) ) ;
#7053 = VECTOR ( 'NONE', #7599, 1000.000000000000000 ) ;
#7054 = CIRCLE ( 'NONE', #353, 2.750000000000002665 ) ;
#7055 = AXIS2_PLACEMENT_3D ( 'NONE', #15242, #6894, #13935 ) ;
#7056 = ORIENTED_EDGE ( 'NONE', *, *, #11805, .F. ) ;
#7057 = EDGE_LOOP ( 'NONE', ( #7080, #1239, #6612, #2982 ) ) ;
#7058 = CARTESIAN_POINT ( 'NONE',  ( -1.914696782014857712, -4.241249999999832987, 2.867854448260448219 ) ) ;
#7059 = VERTEX_POINT ( 'NONE', #2546 ) ;
#7060 = ORIENTED_EDGE ( 'NONE', *, *, #12764, .F. ) ;
#7061 = ADVANCED_FACE ( 'NONE', ( #9373 ), #3560, .F. ) ;
#7062 = EDGE_LOOP ( 'NONE', ( #11934, #1892, #5908, #12811 ) ) ;
#7063 = CARTESIAN_POINT ( 'NONE',  ( -3.491779696971169411, -4.561713562373101993, 1.447843152864476624 ) ) ;
#7064 = DIRECTION ( 'NONE',  ( 0.000000000000000000, 0.000000000000000000, -1.000000000000000000 ) ) ;
#7065 = ADVANCED_FACE ( 'NONE', ( #11864 ), #13791, .T. ) ;
#7066 = DIRECTION ( 'NONE',  ( 0.000000000000000000, 0.000000000000000000, 1.000000000000000000 ) ) ;
#7067 = DIRECTION ( 'NONE',  ( -1.287488025362404182E-15, -1.000000000000000000, 0.000000000000000000 ) ) ;
#7068 = CIRCLE ( 'NONE', #4324, 3.499999999999999556 ) ;
#7069 = CARTESIAN_POINT ( 'NONE',  ( -5.196152422706634688, 1.678847577293359539, -8.911270275552416508E-16 ) ) ;
#7070 = DIRECTION ( 'NONE',  ( 0.000000000000000000, 1.000000000000000000, 0.000000000000000000 ) ) ;
#7071 = CARTESIAN_POINT ( 'NONE',  ( -16.75000000000000000, -2.500000000000000000, 23.22168783648699986 ) ) ;
#7072 = PLANE ( 'NONE',  #128 ) ;
#7073 = CARTESIAN_POINT ( 'NONE',  ( 0.3421672931281763419, -3.819374999999898268, -3.487344533451358863 ) ) ;
#7074 = CARTESIAN_POINT ( 'NONE',  ( 15.50000000000000000, 0.000000000000000000, -18.50000000000000000 ) ) ;
#7075 = EDGE_CURVE ( 'NONE', #6527, #9489, #7296, .T. ) ;
#7076 = ORIENTED_EDGE ( 'NONE', *, *, #1274, .T. ) ;
#7077 = ADVANCED_FACE ( 'NONE', ( #14336 ), #12024, .F. ) ;
#7078 = CARTESIAN_POINT ( 'NONE',  ( -86.77438362643999881, 65.17411849586700612, -150.4984795835770228 ) ) ;
#7079 = ORIENTED_EDGE ( 'NONE', *, *, #876, .T. ) ;
#7080 = ORIENTED_EDGE ( 'NONE', *, *, #13317, .T. ) ;
#7081 = ORIENTED_EDGE ( 'NONE', *, *, #12184, .F. ) ;
#7082 = EDGE_CURVE ( 'NONE', #14576, #12826, #9521, .T. ) ;
#7083 = VECTOR ( 'NONE', #10836, 1000.000000000000000 ) ;
#7084 = AXIS2_PLACEMENT_3D ( 'NONE', #15110, #10384, #624 ) ;
#7085 = CARTESIAN_POINT ( 'NONE',  ( 3.520079602834293109, -3.569375000000153619, 0.3476102605345692265 ) ) ;
#7086 = ADVANCED_FACE ( 'NONE', ( #11938 ), #2396, .F. ) ;
#7087 = ADVANCED_FACE ( 'NONE', ( #7143 ), #11787, .F. ) ;
#7088 = CARTESIAN_POINT ( 'NONE',  ( -16.33565937784311828, -0.3156604612129161880, -23.46090750622545684 ) ) ;
#7089 = CARTESIAN_POINT ( 'NONE',  ( 0.7330380326264336333, -4.781250000000259348, 3.678172007241774732 ) ) ;
#7090 = CARTESIAN_POINT ( 'NONE',  ( -14.25000000000000000, -0.3156864504677174277, 22.74361999681791247 ) ) ;
#7091 = LINE ( 'NONE', #10715, #15001 ) ;
#7092 = CARTESIAN_POINT ( 'NONE',  ( -4.296391350416484123, -0.4995676945082700438, -1.627175273956673067E-05 ) ) ;
#7093 = PRESENTATION_LAYER_ASSIGNMENT (  '', '', ( #9545 ) ) ;
#7094 = LINE ( 'NONE', #9323, #8037 ) ;
#7095 = B_SPLINE_CURVE_WITH_KNOTS ( 'NONE', 3,
 ( #7946, #8889, #13627, #12460 ),
 .UNSPECIFIED., .F., .F.,
 ( 4, 4 ),
 ( 0.006950528372497996078, 0.009557525114560322041 ),
 .UNSPECIFIED. ) ;
#7096 = FACE_OUTER_BOUND ( 'NONE', #14220, .T. ) ;
#7097 = VECTOR ( 'NONE', #11208, 1000.000000000000114 ) ;
#7098 = EDGE_LOOP ( 'NONE', ( #11604, #7483, #1719, #8259 ) ) ;
#7099 = AXIS2_PLACEMENT_3D ( 'NONE', #8906, #6822, #11543 ) ;
#7100 = DIRECTION ( 'NONE',  ( -0.000000000000000000, -0.000000000000000000, 1.000000000000000000 ) ) ;
#7101 = ORIENTED_EDGE ( 'NONE', *, *, #14908, .F. ) ;
#7102 = VERTEX_POINT ( 'NONE', #5987 ) ;
#7103 = EDGE_CURVE ( 'NONE', #10418, #7517, #1305, .T. ) ;
#7104 = ORIENTED_EDGE ( 'NONE', *, *, #598, .F. ) ;
#7105 = CIRCLE ( 'NONE', #7850, 4.499999999999997335 ) ;
#7106 = CARTESIAN_POINT ( 'NONE',  ( -1.246598846679689343, -0.7023385623730667993, 4.105542770413508791 ) ) ;
#7107 = AXIS2_PLACEMENT_3D ( 'NONE', #12981, #14206, #2257 ) ;
#7108 = VECTOR ( 'NONE', #271, 1000.000000000000000 ) ;
#7109 = FACE_OUTER_BOUND ( 'NONE', #14105, .T. ) ;
#7110 = DIRECTION ( 'NONE',  ( 0.000000000000000000, -0.000000000000000000, 1.000000000000000000 ) ) ;
#7111 = DIRECTION ( 'NONE',  ( 0.000000000000000000, 0.000000000000000000, -1.000000000000000000 ) ) ;
#7112 = PRODUCT ( 'Pneumatic Cylinder Piston', 'Pneumatic Cylinder Piston', '', ( #2516 ) ) ;
#7113 = FACE_OUTER_BOUND ( 'NONE', #9865, .T. ) ;
#7114 = ORIENTED_EDGE ( 'NONE', *, *, #14369, .F. ) ;
#7115 = VECTOR ( 'NONE', #2514, 1000.000000000000000 ) ;
#7116 = CARTESIAN_POINT ( 'NONE',  ( -54.81638362644000040, 63.99516924618178848, -147.9984795835769944 ) ) ;
#7117 = CARTESIAN_POINT ( 'NONE',  ( 16.50219555133672955, 11.93237369474095999, 0.2532242768859266357 ) ) ;
#7118 = AXIS2_PLACEMENT_3D ( 'NONE', #14184, #11941, #13956 ) ;
#7119 = EDGE_LOOP ( 'NONE', ( #955, #4700, #9864, #14947, #11065 ) ) ;
#7120 = CARTESIAN_POINT ( 'NONE',  ( -0.3668491701747607636, -4.734375000000160760, 3.738752075031570588 ) ) ;
#7121 = VERTEX_POINT ( 'NONE', #14263 ) ;
#7122 = VECTOR ( 'NONE', #9951, 1000.000000000000000 ) ;
#7123 = CARTESIAN_POINT ( 'NONE',  ( -1.834300037444539511, -0.9131249999999379030, -3.428720741157346374 ) ) ;
#7124 = CARTESIAN_POINT ( 'NONE',  ( 1.682902201845278611, -5.420849775684215999, 2.811263474311217259 ) ) ;
#7125 = AXIS2_PLACEMENT_3D ( 'NONE', #5082, #5729, #8125 ) ;
#7126 = CARTESIAN_POINT ( 'NONE',  ( 15.50000000000000000, -5.000000000000000000, -22.50000000000000000 ) ) ;
#7127 = DIRECTION ( 'NONE',  ( -1.000000000000000000, 0.000000000000000000, -0.000000000000000000 ) ) ;
#7128 = CARTESIAN_POINT ( 'NONE',  ( -13.41835358098578723, 11.99999970914576863, -56.77834603255778489 ) ) ;
#7129 = FACE_BOUND ( 'NONE', #7833, .T. ) ;
#7130 = CARTESIAN_POINT ( 'NONE',  ( -86.77438362644100778, 103.4241184958670061, -145.4984795835769944 ) ) ;
#7131 = CARTESIAN_POINT ( 'NONE',  ( -82.27438362643999881, 99.17411849586700612, -152.4984795835769944 ) ) ;
#7132 = VERTEX_POINT ( 'NONE', #10615 ) ;
#7133 = CARTESIAN_POINT ( 'NONE',  ( -14.25000000000000000, -0.2038245569916330158, -23.22168783648699986 ) ) ;
#7134 =( LENGTH_UNIT ( ) NAMED_UNIT ( * ) SI_UNIT ( .MILLI., .METRE. ) );
#7135 = ADVANCED_FACE ( 'NONE', ( #14848 ), #10535, .F. ) ;
#7136 = ORIENTED_EDGE ( 'NONE', *, *, #1354, .F. ) ;
#7137 = DIRECTION ( 'NONE',  ( 0.000000000000000000, 4.336808689942017736E-16, -1.000000000000000000 ) ) ;
#7138 = CARTESIAN_POINT ( 'NONE',  ( 1.394838545734257140, -2.772499999999996856, -3.364978284447635026 ) ) ;
#7139 = ORIENTED_EDGE ( 'NONE', *, *, #1646, .F. ) ;
#7140 = ORIENTED_EDGE ( 'NONE', *, *, #3195, .T. ) ;
#7141 = ORIENTED_EDGE ( 'NONE', *, *, #13987, .T. ) ;
#7142 = CARTESIAN_POINT ( 'NONE',  ( -2.092043339069166841, -4.655463562372927022, 3.133452599004876493 ) ) ;
#7143 = FACE_OUTER_BOUND ( 'NONE', #1610, .T. ) ;
#7144 = CARTESIAN_POINT ( 'NONE',  ( -52.77438362644100067, 99.17411849586700612, -147.9984795835769944 ) ) ;
#7145 = DIRECTION ( 'NONE',  ( 7.228014483236693351E-17, 1.000000000000000000, 0.000000000000000000 ) ) ;
#7146 = CIRCLE ( 'NONE', #4910, 16.00000000000000000 ) ;
#7147 = DIRECTION ( 'NONE',  ( 1.000000000000000000, 0.000000000000000000, 0.000000000000000000 ) ) ;
#7148 = DIRECTION ( 'NONE',  ( -0.000000000000000000, 1.000000000000000000, -0.000000000000000000 ) ) ;
#7149 = DIRECTION ( 'NONE',  ( 0.000000000000000000, 0.000000000000000000, -1.000000000000000000 ) ) ;
#7150 = ADVANCED_FACE ( 'NONE', ( #9444 ), #14182, .F. ) ;
#7151 = CARTESIAN_POINT ( 'NONE',  ( -2.773226354234704427, -3.194375000000006182, 2.274732928208734961 ) ) ;
#7152 = DIRECTION ( 'NONE',  ( 7.228014483236693351E-17, 1.000000000000000000, 0.000000000000000000 ) ) ;
#7153 = ORIENTED_EDGE ( 'NONE', *, *, #5038, .F. ) ;
#7154 = DIRECTION ( 'NONE',  ( 0.000000000000000000, 1.000000000000000000, 4.336808689942017736E-16 ) ) ;
#7155 = ORIENTED_EDGE ( 'NONE', *, *, #11519, .F. ) ;
#7156 = ORIENTED_EDGE ( 'NONE', *, *, #4313, .F. ) ;
#7157 = EDGE_LOOP ( 'NONE', ( #6683, #2598, #9401, #3457 ) ) ;
#7158 = AXIS2_PLACEMENT_3D ( 'NONE', #2724, #1787, #6625 ) ;
#7159 = CYLINDRICAL_SURFACE ( 'NONE', #6997, 0.9999999999999957812 ) ;
#7160 = CARTESIAN_POINT ( 'NONE',  ( 1.656526992905777318, -3.756875000000012399, -3.097233728230734062 ) ) ;
#7161 = EDGE_CURVE ( 'NONE', #14122, #9136, #14289, .T. ) ;
#7162 = CARTESIAN_POINT ( 'NONE',  ( 3.897114317029974462, 9.945166405816860437E-15, 2.249999999999999556 ) ) ;
#7163 = CARTESIAN_POINT ( 'NONE',  ( 0.000000000000000000, 0.000000000000000000, -79.59847958357700293 ) ) ;
#7164 = CARTESIAN_POINT ( 'NONE',  ( -14.24999999999999822, -0.3152037684892594616, 22.25410949791978510 ) ) ;
#7165 = PLANE ( 'NONE',  #5626 ) ;
#7166 = CARTESIAN_POINT ( 'NONE',  ( -86.77438362644100778, 99.17411849586700612, -150.4984795835770228 ) ) ;
#7167 = CARTESIAN_POINT ( 'NONE',  ( -35.27438362644000591, 60.67411849586700612, -79.49847958357700861 ) ) ;
#7168 = FACE_OUTER_BOUND ( 'NONE', #13296, .T. ) ;
#7169 = EDGE_CURVE ( 'NONE', #3095, #8331, #15260, .T. ) ;
#7170 = PLANE ( 'NONE',  #6360 ) ;
#7171 = CARTESIAN_POINT ( 'NONE',  ( -73.64736697264743270, 75.17411849586699191, -44.99847958359794120 ) ) ;
#7172 = CONICAL_SURFACE ( 'NONE', #3936, 4.500000000000000888, 1.396263401595466691 ) ;
#7173 = ORIENTED_EDGE ( 'NONE', *, *, #14349, .T. ) ;
#7174 = DIRECTION ( 'NONE',  ( 0.000000000000000000, 1.000000000000000000, 0.000000000000000000 ) ) ;
#7175 = EDGE_CURVE ( 'NONE', #13238, #5950, #12877, .T. ) ;
#7176 = EDGE_LOOP ( 'NONE', ( #1336, #9282, #10157, #7687 ) ) ;
#7177 = ADVANCED_FACE ( 'NONE', ( #4656 ), #14110, .F. ) ;
#7178 = EDGE_LOOP ( 'NONE', ( #5171, #7598, #8288, #12017 ) ) ;
#7179 = CARTESIAN_POINT ( 'NONE',  ( 16.75000000000000000, -2.500000000000000000, 21.77831216351300014 ) ) ;
#7180 = B_SPLINE_CURVE_WITH_KNOTS ( 'NONE', 3,
 ( #2800, #7552, #1559, #12351, #1713, #13208 ),
 .UNSPECIFIED., .F., .F.,
 ( 4, 2, 4 ),
 ( 0.0002380763768132232450, 0.7291065797294586925, 1.457975083082104106 ),
 .UNSPECIFIED. ) ;
#7181 = CARTESIAN_POINT ( 'NONE',  ( 4.363871257596563247, 0.01562500000001383962, 0.4309836735954339360 ) ) ;
#7182 = ORIENTED_EDGE ( 'NONE', *, *, #7362, .F. ) ;
#7183 = CARTESIAN_POINT ( 'NONE',  ( -2.023153048893557848, -0.6710885623731100980, 3.788336601472766407 ) ) ;
#7184 = ADVANCED_FACE ( 'NONE', ( #5124 ), #12246, .F. ) ;
#7185 = CARTESIAN_POINT ( 'NONE',  ( 15.50000000000000000, -0.2000000000000000111, 22.50000000000000000 ) ) ;
#7186 = DIRECTION ( 'NONE',  ( -1.000000000000000000, 0.000000000000000000, 0.000000000000000000 ) ) ;
#7187 = CYLINDRICAL_SURFACE ( 'NONE', #10732, 1.500000000000001332 ) ;
#7188 = EDGE_CURVE ( 'NONE', #13728, #6550, #14712, .T. ) ;
#7189 = CARTESIAN_POINT ( 'NONE',  ( -13.41835358098578723, 11.39999970914575833, -0.3335879563140091153 ) ) ;
#7190 = EDGE_LOOP ( 'NONE', ( #5803, #11039, #9664, #11976 ) ) ;
#7191 = CARTESIAN_POINT ( 'NONE',  ( -52.77438362644100067, 99.17411849586700612, -182.2484795835770228 ) ) ;
#7192 = CARTESIAN_POINT ( 'NONE',  ( -1.673688575075003955E-15, 4.650702586819541295, 0.000000000000000000 ) ) ;
#7193 = PRODUCT_DEFINITION_FORMATION_WITH_SPECIFIED_SOURCE ( 'ANY', '', #7112, .NOT_KNOWN. ) ;
#7194 = EDGE_LOOP ( 'NONE', ( #9453, #14532, #9327, #6096 ) ) ;
#7195 = CARTESIAN_POINT ( 'NONE',  ( -79.02077156573416516, 103.6741184958669777, -79.59847958357700293 ) ) ;
#7196 = CARTESIAN_POINT ( 'NONE',  ( 2.153747138339810796, -3.843749999999965361, 3.220761568642789729 ) ) ;
#7197 = EDGE_LOOP ( 'NONE', ( #12237, #1279, #14837, #5403 ) ) ;
#7198 = CARTESIAN_POINT ( 'NONE',  ( -2.135074830120813782, -1.241249999999904707, 3.197897516496418291 ) ) ;
#7199 = LINE ( 'NONE', #10754, #9177 ) ;
#7200 = CARTESIAN_POINT ( 'NONE',  ( -1.442844940792075370, -5.353007078811534036, 3.043495819154527382 ) ) ;
#7201 = FACE_OUTER_BOUND ( 'NONE', #14418, .T. ) ;
#7202 = DIRECTION ( 'NONE',  ( 0.7071067811865474617, 0.000000000000000000, 0.7071067811865474617 ) ) ;
#7203 = DIRECTION ( 'NONE',  ( 1.000000000000000000, 0.000000000000000000, 0.000000000000000000 ) ) ;
#7204 = FACE_OUTER_BOUND ( 'NONE', #301, .T. ) ;
#7205 = FACE_OUTER_BOUND ( 'NONE', #9518, .T. ) ;
#7206 = EDGE_LOOP ( 'NONE', ( #8953, #4987, #9830, #8550, #106 ) ) ;
#7207 = FACE_OUTER_BOUND ( 'NONE', #6351, .T. ) ;
#7208 = ORIENTED_EDGE ( 'NONE', *, *, #12659, .T. ) ;
#7209 = DIRECTION ( 'NONE',  ( -1.000000000000000000, 0.000000000000000000, 0.000000000000000000 ) ) ;
#7210 = CARTESIAN_POINT ( 'NONE',  ( 3.520079602834293553, -3.569375000000153619, 0.3476102605345473551 ) ) ;
#7211 = ORIENTED_EDGE ( 'NONE', *, *, #7472, .T. ) ;
#7212 = EDGE_LOOP ( 'NONE', ( #7706, #3318, #1007, #1966 ) ) ;
#7213 = ORIENTED_EDGE ( 'NONE', *, *, #14564, .F. ) ;
#7214 = DIRECTION ( 'NONE',  ( 1.000000000000000000, -0.000000000000000000, 0.000000000000000000 ) ) ;
#7215 = DIRECTION ( 'NONE',  ( -0.000000000000000000, 0.000000000000000000, 1.000000000000000000 ) ) ;
#7216 = EDGE_CURVE ( 'NONE', #1184, #5656, #11331, .T. ) ;
#7217 = FACE_OUTER_BOUND ( 'NONE', #6721, .T. ) ;
#7218 = AXIS2_PLACEMENT_3D ( 'NONE', #5498, #14858, #14935 ) ;
#7219 = LINE ( 'NONE', #219, #14807 ) ;
#7220 = DIRECTION ( 'NONE',  ( -0.000000000000000000, -1.000000000000000000, -0.000000000000000000 ) ) ;
#7221 = CARTESIAN_POINT ( 'NONE',  ( 3.273328345814555007, -3.522500000000126974, 1.356842221127619874 ) ) ;
#7222 = CARTESIAN_POINT ( 'NONE',  ( -69.77438362644001302, 82.17411849586700612, -80.14847958357698587 ) ) ;
#7223 = ORIENTED_EDGE ( 'NONE', *, *, #8917, .T. ) ;
#7224 = DIRECTION ( 'NONE',  ( -1.000000000000000000, 0.000000000000000000, 0.000000000000000000 ) ) ;
#7225 = VERTEX_POINT ( 'NONE', #2938 ) ;
#7226 = VECTOR ( 'NONE', #10823, 1000.000000000000000 ) ;
#7227 = EDGE_LOOP ( 'NONE', ( #3759, #3576, #5575, #8614 ) ) ;
#7228 = VERTEX_POINT ( 'NONE', #6294 ) ;
#7229 = DIRECTION ( 'NONE',  ( 1.000000000000000000, 0.000000000000000000, 0.000000000000000000 ) ) ;
#7230 = EDGE_CURVE ( 'NONE', #8280, #2251, #15280, .T. ) ;
#7231 = B_SPLINE_SURFACE_WITH_KNOTS ( 'NONE', 1, 3, ( 
 ( #8055, #12498, #6685, #4261, #6910, #11394, #12794, #9138, #4488, #11475, #11323, #691, #841, #12574, #10375, #15100, #5517, #2161, #1935, #7907, #12638, #4194, #613, #5367, #3244, #10075, #10219, #8916, #13733, #14952, #9070, #3024, #13655, #3102, #4345, #13809, #5596, #2003, #6753, #10303, #15031, #13875, #7768, #1857, #5443, #7976, #2083, #6833, #920, #10140, #14032, #10530, #14108, #351, #9811, #12874, #10611, #14541, #1515, #5097, #6978, #14179, #992, #2234, #11782, #9292, #5746, #264, #7427, #11702, #10448, #2312, #4568, #13322, #10984, #6272, #1068, #1227, #15333, #7142, #3923, #4654, #2394, #7063, #5015, #15258, #8648, #2682, #11631, #12146, #13393, #2749, #9370, #1153, #11861, #3404, #5985, #3556, #8140, #5911, #5826, #15179, #3478, #8576, #8212, #8290, #14467, #13033, #12951, #4726, #9730, #9441, #10687, #3850, #12534, #9959, #4161, #8885, #13623, #12310, #2990, #3993, #11364, #14915, #8724, #12456, #731, #7505, #5483, #1597, #10181, #11067, #13993, #9104, #3213, #3368, #10342, #8177, #12907, #13916, #10577, #15068, #10411, #15140, #6722, #11748, #3144, #5787, #11437, #13845, #8101, #1032, #4613, #12677, #15301, #2051, #6873, #7021, #11517, #4384, #4693, #958, #2126, #11662, #12838, #9256, #9405, #9336, #1115, #7943, #6798, #4533, #803, #2273, #5875, #8020, #9174, #7877, #12758, #12610, #1972, #14991, #880, #5643, #6944, #11594, #10495, #5712, #3289, #2201, #4457, #15223, #14075, #3444, #5560, #10262, #2353, #10733, #182, #8557, #6106, #13083, #97, #2667, #8411, #4848, #12134, #2502, #3602, #2436, #8251, #13306, #9710, #10650, #9559, #14303, #251, #1429, #3680, #6185, #9481, #4928, #21, #10966, #11901, #10817, #9637, #4766, #3833, #14371, #13151, #1503, #6255, #12996, #14221, #328, #3749, #5077, #14142, #3517, #10894, #7252, #14446, #11978, #1346, #4997, #8339, #8479, #7106, #7183, #13223, #11828, #2583, #7332, #1193, #12060, #5952, #1262 ),
 ( #6027, #11188, #12436, #10024, #7487, #2819, #7711, #11120, #4144, #7644, #1799, #3978, #12368, #13456, #1659, #8707, #13536, #12519, #3046, #8632, #14756, #7569, #8866, #2974, #1881, #12205, #12287, #6409, #13676, #6636, #11044, #2900, #11347, #14826, #714, #5160, #13606, #14523, #417, #6555, #1580, #3908, #11273, #5393, #9869, #13380, #492, #2736, #637, #8936, #4212, #9790, #6333, #13895, #939, #14054, #13830, #5696, #11497, #3345, #4364, #4589, #1012, #5461, #5766, #3424, #8158, #3199, #15051, #10394, #6706, #15120, #7996, #11414, #4439, #781, #7001, #11727, #2181, #2253, #12736, #8078, #2105, #3124, #7927, #12815, #6776, #4512, #3266, #14894, #14973, #9234, #9088, #2028, #10241, #13753, #9388, #13203, #8537, #12975, #7160, #3, #7393, #1243, #13285, #14351, #4977, #11954, #7085, #1171, #1321, #8315, #6168, #231, #6003, #2647, #13058, #13131, #6085, #4675, #9688, #1093, #3728, #14124, #11806, #10797, #7312, #12040, #5849, #2413, #10553, #9461, #10710, #9538, #3497, #3809, #14200, #75, #4828, #162, #1410, #14282, #8233, #2335, #5930, #10630, #3580, #2954, #2719, #14806, #5288, #9922, #12182, #14502, #1555, #474, #8688, #12417, #5210, #5369, #6387, #6311, #8918, #11020, #14655, #614, #5139, #13363, #13656, #4038, #8767, #10000, #7623, #2878, #3026, #1781, #12117, #7464, #394, #13510, #304, #6234, #10943, #1636, #2794, #5054, #12345, #9767, #3889, #9850, #3962, #7548, #14730, #1708, #4121, #6459, #12265, #11169, #6686, #11395, #13951, #760, #2004, #11324, #692, #4346, #9139, #2162, #15032, #5518, #9071, #11632, #6755, #13811, #5747, #11476, #12575, #10220, #1859, #6911, #3325, #4263, #3178, #12639, #9212, #10377, #842, #15101, #3104, #13876, #8991, #4569, #14953, #4420, #3245, #13734, #12796, #7978, #5598, #10450, #994, #6617, #1936, #15180, #12714, #14034, #7769, #12499, #4489, #10305, #8056, #2084, #6835, #5444, #11557, #921, #10141, #5681 ) ),
 .UNSPECIFIED., .F., .F., .F.,
 ( 2, 2 ),
 ( 4, 2, 2, 2, 2, 2, 2, 2, 2, 2, 2, 2, 2, 2, 2, 2, 2, 2, 2, 2, 2, 2, 2, 2, 2, 2, 2, 2, 2, 2, 2, 2, 2, 2, 2, 2, 2, 2, 2, 2, 2, 2, 2, 2, 2, 2, 2, 2, 2, 2, 2, 2, 2, 2, 2, 2, 2, 2, 2, 2, 2, 2, 2, 2, 2, 2, 2, 2, 2, 2, 2, 2, 2, 2, 2, 2, 2, 2, 2, 2, 2, 2, 2, 2, 2, 2, 2, 2, 2, 2, 2, 2, 2, 2, 2, 2, 2, 2, 2, 2, 2, 2, 2, 2, 2, 2, 2, 2, 2, 2, 2, 2, 2, 2, 2, 2, 2, 2, 2, 2, 2, 2, 2, 2, 2, 2, 2, 2, 4 ),
 ( 0.000000000000000000, 1.000000000000000000 ),
 ( 0.000000000000000000, 0.007812500000000000000, 0.01562500000000000000, 0.02343750000000000000, 0.03125000000000000000, 0.03906250000000000000, 0.04687500000000000000, 0.05468750000000000000, 0.06250000000000000000, 0.07031250000000000000, 0.07812500000000000000, 0.08593750000000000000, 0.09375000000000000000, 0.1015625000000000000, 0.1093750000000000000, 0.1171875000000000000, 0.1250000000000000000, 0.1328125000000000000, 0.1406250000000000000, 0.1484375000000000000, 0.1562500000000000000, 0.1640625000000000000, 0.1718750000000000000, 0.1796875000000000000, 0.1875000000000000000, 0.1953125000000000000, 0.2031250000000000000, 0.2109375000000000000, 0.2187500000000000000, 0.2265625000000000000, 0.2343750000000000000, 0.2421875000000000000, 0.2500000000000000000, 0.2578125000000000000, 0.2656250000000000000, 0.2734375000000000000, 0.2812500000000000000, 0.2890625000000000000, 0.2968750000000000000, 0.3046875000000000000, 0.3125000000000000000, 0.3203125000000000000, 0.3281250000000000000, 0.3359375000000000000, 0.3437500000000000000, 0.3515625000000000000, 0.3593750000000000000, 0.3671875000000000000, 0.3750000000000000000, 0.3828125000000000000, 0.3906250000000000000, 0.3984375000000000000, 0.4062500000000000000, 0.4140625000000000000, 0.4218750000000000000, 0.4296875000000000000, 0.4375000000000000000, 0.4453125000000000000, 0.4531250000000000000, 0.4609375000000000000, 0.4687500000000000000, 0.4765625000000000000, 0.4843750000000000000, 0.4921875000000000000, 0.5000000000000000000, 0.5078125000000000000, 0.5156250000000000000, 0.5234375000000000000, 0.5312500000000000000, 0.5390625000000000000, 0.5468750000000000000, 0.5546875000000000000, 0.5625000000000000000, 0.5703125000000000000, 0.5781250000000000000, 0.5859375000000000000, 0.5937500000000000000, 0.6015625000000000000, 0.6093750000000000000, 0.6171875000000000000, 0.6250000000000000000, 0.6328125000000000000, 0.6406250000000000000, 0.6484375000000000000, 0.6562500000000000000, 0.6640625000000000000, 0.6718750000000000000, 0.6796875000000000000, 0.6875000000000000000, 0.6953125000000000000, 0.7031250000000000000, 0.7109375000000000000, 0.7187500000000000000, 0.7265625000000000000, 0.7343750000000000000, 0.7421875000000000000, 0.7500000000000000000, 0.7578125000000000000, 0.7656250000000000000, 0.7734375000000000000, 0.7812500000000000000, 0.7890625000000000000, 0.7968750000000000000, 0.8046875000000000000, 0.8125000000000000000, 0.8203125000000000000, 0.8281250000000000000, 0.8359375000000000000, 0.8437500000000000000, 0.8515625000000000000, 0.8593750000000000000, 0.8671875000000000000, 0.8750000000000000000, 0.8828125000000000000, 0.8906250000000000000, 0.8984375000000000000, 0.9062500000000000000, 0.9140625000000000000, 0.9218750000000000000, 0.9296875000000000000, 0.9375000000000000000, 0.9453125000000000000, 0.9531250000000000000, 0.9609375000000000000, 0.9687500000000000000, 0.9765625000000000000, 0.9843750000000000000, 0.9921875000000000000, 1.000000000000000000 ),
 .UNSPECIFIED. ) ;
#7232 = FACE_OUTER_BOUND ( 'NONE', #3322, .T. ) ;
#7233 = PLANE ( 'NONE',  #10188 ) ;
#7234 = FACE_OUTER_BOUND ( 'NONE', #1064, .T. ) ;
#7235 = ADVANCED_FACE ( 'NONE', ( #8671 ), #7872, .F. ) ;
#7236 = CARTESIAN_POINT ( 'NONE',  ( 15.50000000000000000, -1.037157890325000054, -19.00000000000000000 ) ) ;
#7237 = DIRECTION ( 'NONE',  ( 1.000000000000000000, 0.000000000000000000, 0.000000000000000000 ) ) ;
#7238 = CARTESIAN_POINT ( 'NONE',  ( -86.77438362644001302, 82.17411849586700612, -81.84847958357697451 ) ) ;
#7239 = CARTESIAN_POINT ( 'NONE',  ( 15.50000000000000000, -2.500000000000000000, 21.05662432702600029 ) ) ;
#7240 = CARTESIAN_POINT ( 'NONE',  ( -15.08757311576351334, -0.3152598339557977081, -21.29473909966096556 ) ) ;
#7241 = DIRECTION ( 'NONE',  ( 0.8660254037844387076, 0.4999999999999998890, 0.000000000000000000 ) ) ;
#7242 = ORIENTED_EDGE ( 'NONE', *, *, #1173, .T. ) ;
#7243 = CARTESIAN_POINT ( 'NONE',  ( 22.58164641901421632, -12.00000029085423670, -11.73358795631400930 ) ) ;
#7244 = AXIS2_PLACEMENT_3D ( 'NONE', #9128, #9360, #8200 ) ;
#7245 = EDGE_LOOP ( 'NONE', ( #14334, #3020 ) ) ;
#7246 = VERTEX_POINT ( 'NONE', #13414 ) ;
#7247 = VERTEX_POINT ( 'NONE', #6372 ) ;
#7248 = DIRECTION ( 'NONE',  ( -2.551930889570660354E-15, 1.000000000000000000, 0.000000000000000000 ) ) ;
#7249 = AXIS2_PLACEMENT_3D ( 'NONE', #15053, #7931, #11646 ) ;
#7250 = ORIENTED_EDGE ( 'NONE', *, *, #3843, .T. ) ;
#7251 = EDGE_CURVE ( 'NONE', #11935, #7479, #11940, .T. ) ;
#7252 = CARTESIAN_POINT ( 'NONE',  ( 2.709998298289202356, -0.8585885623730556970, 3.299714903563142787 ) ) ;
#7253 = VECTOR ( 'NONE', #1092, 1000.000000000000000 ) ;
#7254 = DIRECTION ( 'NONE',  ( 0.000000000000000000, 0.000000000000000000, 1.000000000000000000 ) ) ;
#7255 = AXIS2_PLACEMENT_3D ( 'NONE', #12686, #13005, #9266 ) ;
#7256 = ADVANCED_FACE ( 'NONE', ( #13493 ), #2857, .F. ) ;
#7257 = DIRECTION ( 'NONE',  ( 0.000000000000000000, 0.000000000000000000, 1.000000000000000000 ) ) ;
#7258 = CARTESIAN_POINT ( 'NONE',  ( 4.463089466550662188, 2.239389106484356518, -1.269702285208761605 ) ) ;
#7259 = AXIS2_PLACEMENT_3D ( 'NONE', #3230, #11462, #12782 ) ;
#7260 = CARTESIAN_POINT ( 'NONE',  ( -61.59970400812709102, 70.01464610989972925, -83.44847958357698303 ) ) ;
#7261 = ORIENTED_EDGE ( 'NONE', *, *, #6513, .T. ) ;
#7262 = CARTESIAN_POINT ( 'NONE',  ( -84.73238362644100619, 100.3530677455522238, -150.4984795835770228 ) ) ;
#7263 = CARTESIAN_POINT ( 'NONE',  ( -60.43728955831366534, 68.38713492810558137, -81.84847958357697451 ) ) ;
#7264 = EDGE_CURVE ( 'NONE', #2695, #8820, #8828, .T. ) ;
#7265 = EDGE_CURVE ( 'NONE', #10774, #1225, #12328, .T. ) ;
#7266 = VECTOR ( 'NONE', #5447, 1000.000000000000000 ) ;
#7267 = PRODUCT_CONTEXT ( 'NONE', #289, 'mechanical' ) ;
#7268 = ORIENTED_EDGE ( 'NONE', *, *, #1916, .F. ) ;
#7269 = SURFACE_STYLE_FILL_AREA ( #7348 ) ;
#7270 = CARTESIAN_POINT ( 'NONE',  ( -3.771471614353887336, -4.484375000000117240, -0.3724498170710106582 ) ) ;
#7271 = ORIENTED_EDGE ( 'NONE', *, *, #6742, .T. ) ;
#7272 = EDGE_CURVE ( 'NONE', #8742, #1753, #1987, .T. ) ;
#7273 = AXIS2_PLACEMENT_3D ( 'NONE', #2189, #11816, #9471 ) ;
#7274 = CARTESIAN_POINT ( 'NONE',  ( -69.77438362644001302, 84.67411849586700612, -67.69567958357700377 ) ) ;
#7275 = EDGE_CURVE ( 'NONE', #15133, #3902, #7959, .T. ) ;
#7276 = CARTESIAN_POINT ( 'NONE',  ( -75.01311196519617397, 67.29799558322736175, -83.44847958357698303 ) ) ;
#7277 = ADVANCED_FACE ( 'NONE', ( #6818 ), #11458, .T. ) ;
#7278 = CIRCLE ( 'NONE', #9978, 2.042000000000002036 ) ;
#7279 = DIRECTION ( 'NONE',  ( 0.000000000000000000, 0.000000000000000000, 1.000000000000000000 ) ) ;
#7280 = CIRCLE ( 'NONE', #11473, 8.349999999999996092 ) ;
#7281 = DIRECTION ( 'NONE',  ( -1.000000000000000000, 0.000000000000000000, 0.000000000000000000 ) ) ;
#7282 = CARTESIAN_POINT ( 'NONE',  ( 2.811606400754406820, -5.337890745103998746, 1.889891293729461186 ) ) ;
#7283 = PLANE ( 'NONE',  #12296 ) ;
#7284 = CARTESIAN_POINT ( 'NONE',  ( -16.75000000000000000, -2.500000000000000000, -21.77831216351300014 ) ) ;
#7285 = AXIS2_PLACEMENT_3D ( 'NONE', #2094, #7917, #5609 ) ;
#7286 = VERTEX_POINT ( 'NONE', #8975 ) ;
#7287 = CARTESIAN_POINT ( 'NONE',  ( -69.77438362644001302, 82.17411849586700612, -80.44847958357698303 ) ) ;
#7288 = ORIENTED_EDGE ( 'NONE', *, *, #10171, .F. ) ;
#7289 = DIRECTION ( 'NONE',  ( 0.9961946980917452121, -7.200509705930739692E-17, 0.08715574274766157981 ) ) ;
#7290 = CARTESIAN_POINT ( 'NONE',  ( -3.581969766213484618, -3.100624999999847198, 0.3518610084922548231 ) ) ;
#7291 = EDGE_LOOP ( 'NONE', ( #5842, #13501, #740, #9367 ) ) ;
#7292 = EDGE_LOOP ( 'NONE', ( #13807, #6105, #5996, #4843 ) ) ;
#7293 = VECTOR ( 'NONE', #8465, 1000.000000000000000 ) ;
#7294 = AXIS2_PLACEMENT_3D ( 'NONE', #4737, #7154, #7832 ) ;
#7295 = VERTEX_POINT ( 'NONE', #14936 ) ;
#7296 = LINE ( 'NONE', #1155, #8350 ) ;
#7297 = DIRECTION ( 'NONE',  ( 0.000000000000000000, -0.000000000000000000, 1.000000000000000000 ) ) ;
#7298 = CARTESIAN_POINT ( 'NONE',  ( -0.8000000000000114797, 9.500000000000000000, 0.000000000000000000 ) ) ;
#7299 = DIRECTION ( 'NONE',  ( 0.000000000000000000, 1.000000000000000000, 0.000000000000000000 ) ) ;
#7300 = VECTOR ( 'NONE', #9210, 1000.000000000000000 ) ;
#7301 = TOROIDAL_SURFACE ( 'NONE', #13245, 2.931404194366992400, 0.5000000000000000000 ) ;
#7302 = CARTESIAN_POINT ( 'NONE',  ( -3.468991550463924156, -4.085000000000062137, -0.0008868951686453910126 ) ) ;
#7303 = CARTESIAN_POINT ( 'NONE',  ( -52.77438362644000591, 65.17411849586700612, -86.49847958357699440 ) ) ;
#7304 = ORIENTED_EDGE ( 'NONE', *, *, #8372, .T. ) ;
#7305 = DIRECTION ( 'NONE',  ( 0.000000000000000000, 0.000000000000000000, -1.000000000000000000 ) ) ;
#7306 = EDGE_LOOP ( 'NONE', ( #10900, #487, #5301, #2660 ) ) ;
#7307 = VERTEX_POINT ( 'NONE', #4473 ) ;
#7308 = ORIENTED_EDGE ( 'NONE', *, *, #5738, .F. ) ;
#7309 = ORIENTED_EDGE ( 'NONE', *, *, #4281, .T. ) ;
#7310 = DIRECTION ( 'NONE',  ( 0.000000000000000000, -1.000000000000000000, 0.000000000000000000 ) ) ;
#7311 = AXIS2_PLACEMENT_3D ( 'NONE', #4901, #9606, #3719 ) ;
#7312 = CARTESIAN_POINT ( 'NONE',  ( -3.319861881881159160, -3.147500000000079456, 1.374129751973758307 ) ) ;
#7313 = CIRCLE ( 'NONE', #7806, 3.000000000000000888 ) ;
#7314 = CARTESIAN_POINT ( 'NONE',  ( -1.438726384651785040, -4.687499999999733546, 3.477001582427886817 ) ) ;
#7315 = CARTESIAN_POINT ( 'NONE',  ( -9.797174393178927223E-17, 9.500000000000000000, 0.000000000000000000 ) ) ;
#7316 = FACE_OUTER_BOUND ( 'NONE', #8244, .T. ) ;
#7317 = CYLINDRICAL_SURFACE ( 'NONE', #8864, 1.999999999999988010 ) ;
#7318 = DIRECTION ( 'NONE',  ( 0.000000000000000000, 0.000000000000000000, -1.000000000000000000 ) ) ;
#7319 = LINE ( 'NONE', #11963, #7578 ) ;
#7320 = CARTESIAN_POINT ( 'NONE',  ( -62.02799568714584666, 103.6741184958669919, -73.34256232478206528 ) ) ;
#7321 = DIRECTION ( 'NONE',  ( 0.000000000000000000, -1.000000000000000000, 0.000000000000000000 ) ) ;
#7322 = VERTEX_POINT ( 'NONE', #825 ) ;
#7323 = DIRECTION ( 'NONE',  ( 0.000000000000000000, 0.000000000000000000, 1.000000000000000000 ) ) ;
#7324 = ADVANCED_FACE ( 'NONE', ( #12558 ), #5427, .T. ) ;
#7325 = VERTEX_POINT ( 'NONE', #5347 ) ;
#7326 = CIRCLE ( 'NONE', #9281, 4.250000000000003553 ) ;
#7327 = ORIENTED_EDGE ( 'NONE', *, *, #13303, .T. ) ;
#7328 = CIRCLE ( 'NONE', #10521, 2.042000000000002036 ) ;
#7329 = DIRECTION ( 'NONE',  ( 1.000000000000000000, 2.551930889570660354E-15, 0.000000000000000000 ) ) ;
#7330 = EDGE_CURVE ( 'NONE', #2695, #3825, #6650, .T. ) ;
#7331 = CARTESIAN_POINT ( 'NONE',  ( -0.8607816759752345837, 0.2812500000001324496, 4.335577264497109340 ) ) ;
#7332 = CARTESIAN_POINT ( 'NONE',  ( -3.797812870634804217, -0.5773385623730058480, 2.031732732842940425 ) ) ;
#7333 = CARTESIAN_POINT ( 'NONE',  ( 40.52020888806953991, 0.000000000000000000, 6.000000000000000000 ) ) ;
#7334 = DIRECTION ( 'NONE',  ( 1.000000000000000000, 0.000000000000000000, 0.000000000000000000 ) ) ;
#7335 = DIRECTION ( 'NONE',  ( 1.000000000000000000, 0.000000000000000000, 0.000000000000000000 ) ) ;
#7336 = VECTOR ( 'NONE', #3326, 1000.000000000000000 ) ;
#7337 = PLANE ( 'NONE',  #12978 ) ;
#7338 = VECTOR ( 'NONE', #2636, 1000.000000000000000 ) ;
#7339 = FACE_OUTER_BOUND ( 'NONE', #11803, .T. ) ;
#7340 = ORIENTED_EDGE ( 'NONE', *, *, #7747, .T. ) ;
#7341 = EDGE_CURVE ( 'NONE', #13910, #12014, #3160, .T. ) ;
#7342 = FACE_BOUND ( 'NONE', #4820, .T. ) ;
#7343 = EDGE_CURVE ( 'NONE', #9479, #6326, #676, .T. ) ;
#7344 = CIRCLE ( 'NONE', #3613, 4.000000000000001776 ) ;
#7345 = APPLICATION_PROTOCOL_DEFINITION ( 'draft international standard', 'automotive_design', 1998, #10906 ) ;
#7346 = EDGE_LOOP ( 'NONE', ( #9030, #3191, #10704, #7461 ) ) ;
#7347 = CIRCLE ( 'NONE', #642, 16.06499999999999773 ) ;
#7348 = FILL_AREA_STYLE ('',( #15314 ) ) ;
#7349 = CARTESIAN_POINT ( 'NONE',  ( -3.898923295066525352, -3.515625000000077716, 0.3854469994812330658 ) ) ;
#7350 = EDGE_LOOP ( 'NONE', ( #9555, #8309, #14596 ) ) ;
#7351 = AXIS2_PLACEMENT_3D ( 'NONE', #12087, #4878, #13252 ) ;
#7352 = CARTESIAN_POINT ( 'NONE',  ( -3.795858268372354516, -1.053749999999936460, -0.7536008350790791566 ) ) ;
#7353 = CARTESIAN_POINT ( 'NONE',  ( -15.50000000000000000, -0.2000000000000000111, -19.20000000000052509 ) ) ;
#7354 = EDGE_CURVE ( 'NONE', #384, #6165, #7631, .T. ) ;
#7355 = CIRCLE ( 'NONE', #651, 2.500000000000002220 ) ;
#7356 = FACE_OUTER_BOUND ( 'NONE', #6454, .T. ) ;
#7357 = CIRCLE ( 'NONE', #7839, 4.000000000000000000 ) ;
#7358 = CARTESIAN_POINT ( 'NONE',  ( -69.77438362644002723, 75.17411849587348627, -43.99847958364158984 ) ) ;
#7359 = CYLINDRICAL_SURFACE ( 'NONE', #14185, 4.500000000000003553 ) ;
#7360 = DIRECTION ( 'NONE',  ( -0.9999934663667179313, 1.567696289299852222E-18, -0.003614861529252313445 ) ) ;
#7361 = CARTESIAN_POINT ( 'NONE',  ( 11.02010870769206541, -11.00000029085428110, 70.09311034953164210 ) ) ;
#7362 = EDGE_CURVE ( 'NONE', #1952, #10812, #9122, .T. ) ;
#7363 = DIRECTION ( 'NONE',  ( 1.000000000000000000, 0.000000000000000000, 0.000000000000000000 ) ) ;
#7364 = ORIENTED_EDGE ( 'NONE', *, *, #12068, .F. ) ;
#7365 = CARTESIAN_POINT ( 'NONE',  ( -15.50000000000000000, -1.037157890325000054, -26.50000000000000000 ) ) ;
#7366 = ORIENTED_EDGE ( 'NONE', *, *, #9893, .T. ) ;
#7367 = ADVANCED_FACE ( 'NONE', ( #5661 ), #914, .F. ) ;
#7368 = DIRECTION ( 'NONE',  ( 1.000000000000000000, 0.000000000000000000, 0.000000000000000000 ) ) ;
#7369 = ADVANCED_FACE ( 'NONE', ( #15086 ), #1172, .T. ) ;
#7370 = CARTESIAN_POINT ( 'NONE',  ( -2.773226354234704427, -3.194375000000006182, 2.274732928208646587 ) ) ;
#7371 = ORIENTED_EDGE ( 'NONE', *, *, #14059, .F. ) ;
#7372 = VECTOR ( 'NONE', #7029, 1000.000000000000114 ) ;
#7373 = ORIENTED_EDGE ( 'NONE', *, *, #11682, .F. ) ;
#7374 = ORIENTED_EDGE ( 'NONE', *, *, #9789, .T. ) ;
#7375 = AXIS2_PLACEMENT_3D ( 'NONE', #3732, #10947, #8463 ) ;
#7376 = DIRECTION ( 'NONE',  ( -0.7071067811865474617, 8.659560562354921765E-17, 0.7071067811865474617 ) ) ;
#7377 = ADVANCED_FACE ( 'NONE', ( #7201 ), #3462, .T. ) ;
#7378 = DIRECTION ( 'NONE',  ( 1.000000000000000000, 0.000000000000000000, 0.000000000000000000 ) ) ;
#7379 = PLANE ( 'NONE',  #2581 ) ;
#7380 = PLANE ( 'NONE',  #2179 ) ;
#7381 = CARTESIAN_POINT ( 'NONE',  ( 14.45313394609757296, -0.2715358723599907709, -21.66103272505201005 ) ) ;
#7382 = DIRECTION ( 'NONE',  ( 0.7071067811865474617, 0.000000000000000000, 0.7071067811865474617 ) ) ;
#7383 = ADVANCED_FACE ( 'NONE', ( #13384 ), #9580, .F. ) ;
#7384 = LINE ( 'NONE', #11091, #13229 ) ;
#7385 = VECTOR ( 'NONE', #3390, 1000.000000000000000 ) ;
#7386 = EDGE_LOOP ( 'NONE', ( #11359, #4652 ) ) ;
#7387 = CYLINDRICAL_SURFACE ( 'NONE', #12218, 8.124999999999992895 ) ;
#7388 = ORIENTED_EDGE ( 'NONE', *, *, #8222, .T. ) ;
#7389 = VERTEX_POINT ( 'NONE', #8194 ) ;
#7390 = ORIENTED_EDGE ( 'NONE', *, *, #7580, .F. ) ;
#7391 = ORIENTED_EDGE ( 'NONE', *, *, #3174, .F. ) ;
#7392 = LINE ( 'NONE', #12116, #5576 ) ;
#7393 = CARTESIAN_POINT ( 'NONE',  ( 2.488663048653545928, -3.709999999999854303, -2.487386788893799494 ) ) ;
#7394 = CIRCLE ( 'NONE', #7643, 3.749999999999996447 ) ;
#7395 = CYLINDRICAL_SURFACE ( 'NONE', #15226, 3.499999999999999556 ) ;
#7396 = CARTESIAN_POINT ( 'NONE',  ( -2.390027884620886667, -4.640624999999809042, 2.914437415443186907 ) ) ;
#7397 = CARTESIAN_POINT ( 'NONE',  ( -38.27438362644000591, 60.67411849586700612, 0.000000000000000000 ) ) ;
#7398 = DIRECTION ( 'NONE',  ( -0.000000000000000000, -0.000000000000000000, 1.000000000000000000 ) ) ;
#7399 = LINE ( 'NONE', #10717, #11842 ) ;
#7400 = DIRECTION ( 'NONE',  ( -0.000000000000000000, -0.000000000000000000, 1.000000000000000000 ) ) ;
#7401 = FACE_OUTER_BOUND ( 'NONE', #3954, .T. ) ;
#7402 = DIRECTION ( 'NONE',  ( 0.000000000000000000, 1.000000000000000000, 0.000000000000000000 ) ) ;
#7403 = DIRECTION ( 'NONE',  ( 0.000000000000000000, 0.000000000000000000, 1.000000000000000000 ) ) ;
#7404 = ORIENTED_EDGE ( 'NONE', *, *, #8500, .F. ) ;
#7405 = DIRECTION ( 'NONE',  ( 0.000000000000000000, 0.000000000000000000, 1.000000000000000000 ) ) ;
#7406 = ORIENTED_EDGE ( 'NONE', *, *, #9043, .T. ) ;
#7407 = VECTOR ( 'NONE', #11174, 1000.000000000000000 ) ;
#7408 = ORIENTED_EDGE ( 'NONE', *, *, #13152, .T. ) ;
#7409 = CARTESIAN_POINT ( 'NONE',  ( -3.322613055092911605, -5.069375000000116316, -0.3280989749989033366 ) ) ;
#7410 = CARTESIAN_POINT ( 'NONE',  ( -71.13655333277205273, 90.17411849586699191, -58.99847958357693756 ) ) ;
#7411 = B_SPLINE_CURVE_WITH_KNOTS ( 'NONE', 3,
 ( #8748, #13494, #1306, #9599 ),
 .UNSPECIFIED., .F., .F.,
 ( 4, 4 ),
 ( 2.309401076760371583E-07, 0.002598307151460989804 ),
 .UNSPECIFIED. ) ;
#7412 = DIRECTION ( 'NONE',  ( 1.000000000000000000, 0.000000000000000000, 0.000000000000000000 ) ) ;
#7413 = CARTESIAN_POINT ( 'NONE',  ( -55.27438362643999881, 65.17411849586700612, -79.59847958357700293 ) ) ;
#7414 = SPHERICAL_SURFACE ( 'NONE', #15257, 0.8600000000000014300 ) ;
#7415 = CIRCLE ( 'NONE', #1205, 2.500000000000002220 ) ;
#7416 = DIRECTION ( 'NONE',  ( 0.000000000000000000, 0.000000000000000000, -1.000000000000000000 ) ) ;
#7417 = EDGE_CURVE ( 'NONE', #3798, #5961, #14055, .T. ) ;
#7418 = DIRECTION ( 'NONE',  ( 0.9961946980917453232, -7.200509705930739692E-17, 0.08715574274766157981 ) ) ;
#7419 = EDGE_LOOP ( 'NONE', ( #9950, #11466, #8932, #1649, #7371, #8226, #10069, #12090 ) ) ;
#7420 = PLANE ( 'NONE',  #12566 ) ;
#7421 = CONTEXT_DEPENDENT_SHAPE_REPRESENTATION ( #3769, #2510 ) ;
#7422 = VERTEX_POINT ( 'NONE', #9275 ) ;
#7423 = CIRCLE ( 'NONE', #5953, 2.042000000000002036 ) ;
#7424 = PRESENTATION_STYLE_ASSIGNMENT (( #5091 ) ) ;
#7425 = CARTESIAN_POINT ( 'NONE',  ( 1.111882196364886832, -4.203124999999903189, -3.661942331401731199 ) ) ;
#7426 = EDGE_LOOP ( 'NONE', ( #2866, #9972 ) ) ;
#7427 = CARTESIAN_POINT ( 'NONE',  ( 3.291357201573688496, -4.921088562373032715, 1.760366434726516660 ) ) ;
#7428 = PRODUCT_DEFINITION ( 'UNKNOWN', '', #2975, #7642 ) ;
#7429 = CARTESIAN_POINT ( 'NONE',  ( 2.949251946438511407, -1.475624999999980647, 2.418581166398158455 ) ) ;
#7430 = EDGE_CURVE ( 'NONE', #1293, #12917, #3398, .T. ) ;
#7431 = DIRECTION ( 'NONE',  ( 0.000000000000000000, 0.000000000000000000, 1.000000000000000000 ) ) ;
#7432 = DIRECTION ( 'NONE',  ( -0.08715574274766167695, 0.000000000000000000, 0.9961946980917453232 ) ) ;
#7433 = CARTESIAN_POINT ( 'NONE',  ( 14.25000000000000000, -0.2038245569916330158, -21.77831216351300014 ) ) ;
#7434 = EDGE_CURVE ( 'NONE', #6249, #2847, #14788, .T. ) ;
#7435 = DIRECTION ( 'NONE',  ( -1.000000000000000000, -0.000000000000000000, -0.000000000000000000 ) ) ;
#7436 = DIRECTION ( 'NONE',  ( 0.000000000000000000, -0.000000000000000000, 1.000000000000000000 ) ) ;
#7437 = DIRECTION ( 'NONE',  ( -1.000000000000000000, 0.000000000000000000, 0.000000000000000000 ) ) ;
#7438 = DIRECTION ( 'NONE',  ( 0.000000000000000000, -0.000000000000000000, 1.000000000000000000 ) ) ;
#7439 = VERTEX_POINT ( 'NONE', #3625 ) ;
#7440 = EDGE_LOOP ( 'NONE', ( #5134, #13110, #10467 ) ) ;
#7441 = DIRECTION ( 'NONE',  ( 0.000000000000000000, 0.000000000000000000, 1.000000000000000000 ) ) ;
#7442 = ORIENTED_EDGE ( 'NONE', *, *, #3091, .F. ) ;
#7443 = CYLINDRICAL_SURFACE ( 'NONE', #101, 4.000000000000004441 ) ;
#7444 = CARTESIAN_POINT ( 'NONE',  ( -3.319861881881159604, -3.147500000000079456, 1.374129751973758529 ) ) ;
#7445 = ORIENTED_EDGE ( 'NONE', *, *, #894, .T. ) ;
#7446 = EDGE_LOOP ( 'NONE', ( #2384, #14748 ) ) ;
#7447 = FACE_OUTER_BOUND ( 'NONE', #6701, .T. ) ;
#7448 = EDGE_CURVE ( 'NONE', #13359, #9306, #8609, .T. ) ;
#7449 = CARTESIAN_POINT ( 'NONE',  ( 2.674318815604713073, -5.110407362173572388, -2.536235381543390677 ) ) ;
#7450 = DIRECTION ( 'NONE',  ( 0.000000000000000000, 1.000000000000000000, 4.336808689942017736E-16 ) ) ;
#7451 = EDGE_CURVE ( 'NONE', #11316, #10367, #9422, .T. ) ;
#7452 = CARTESIAN_POINT ( 'NONE',  ( 3.800285711464508331, -0.4995676945082491160, -1.326881515511059817 ) ) ;
#7453 = FACE_OUTER_BOUND ( 'NONE', #11319, .T. ) ;
#7454 = CARTESIAN_POINT ( 'NONE',  ( -59.27438362644000591, 82.17411849586700612, -182.1969643934119745 ) ) ;
#7455 = DIRECTION ( 'NONE',  ( -0.000000000000000000, 0.000000000000000000, 1.000000000000000000 ) ) ;
#7456 = ORIENTED_EDGE ( 'NONE', *, *, #4895, .F. ) ;
#7457 = DIRECTION ( 'NONE',  ( -1.000000000000000000, -1.084202172485497334E-15, 0.000000000000000000 ) ) ;
#7458 = ORIENTED_EDGE ( 'NONE', *, *, #13994, .T. ) ;
#7459 = EDGE_CURVE ( 'NONE', #3281, #9205, #10596, .T. ) ;
#7460 = ORIENTED_EDGE ( 'NONE', *, *, #13577, .T. ) ;
#7461 = ORIENTED_EDGE ( 'NONE', *, *, #9200, .F. ) ;
#7462 = ORIENTED_EDGE ( 'NONE', *, *, #7986, .F. ) ;
#7463 = CARTESIAN_POINT ( 'NONE',  ( 15.50000000000000000, -0.4000000000000000222, 22.50000000000000000 ) ) ;
#7464 = CARTESIAN_POINT ( 'NONE',  ( -2.381388125886219509, -1.944375000000168052, -2.899558211763606064 ) ) ;
#7465 = EDGE_CURVE ( 'NONE', #1114, #9632, #674, .T. ) ;
#7466 = B_SPLINE_CURVE_WITH_KNOTS ( 'NONE', 3,
 ( #2999, #6582, #4169, #665, #7671, #6728, #6808, #11216, #5418, #13633, #5649, #10119, #11524, #3154, #3218, #10193, #5333, #14782 ),
 .UNSPECIFIED., .F., .F.,
 ( 4, 2, 2, 2, 2, 2, 2, 2, 4 ),
 ( 0.01135168602782440743, 0.01221517698400053330, 0.01307866794017665917, 0.01394215889635278677, 0.01480564985252891264, 0.01566914080870503850, 0.01653263176488116437, 0.01739612272105729024, 0.01825961367723341611 ),
 .UNSPECIFIED. ) ;
#7467 = FILL_AREA_STYLE_COLOUR ( '', #5338 ) ;
#7468 = CARTESIAN_POINT ( 'NONE',  ( -3.898923295066525352, -3.515625000000077716, 0.3854469994812330658 ) ) ;
#7469 = CARTESIAN_POINT ( 'NONE',  ( -86.77438362644100778, 99.17411849586700612, -150.4984795835770228 ) ) ;
#7470 = PLANE ( 'NONE',  #4369 ) ;
#7471 = ADVANCED_FACE ( 'NONE', ( #11845 ), #1212, .F. ) ;
#7472 = EDGE_CURVE ( 'NONE', #10684, #8823, #12138, .T. ) ;
#7473 = CARTESIAN_POINT ( 'NONE',  ( -2.801070059014840741, 1.881841424954886710, -4.148404342226347019 ) ) ;
#7474 = CARTESIAN_POINT ( 'NONE',  ( 2.431404194366990623, 4.650702586819541295, 2.977611364064985881E-16 ) ) ;
#7475 = CARTESIAN_POINT ( 'NONE',  ( 3.173335668876534843, -5.499999999999995559, 3.886215369509756487E-16 ) ) ;
#7476 = DIRECTION ( 'NONE',  ( 0.5000000000000002220, 0.000000000000000000, 0.8660254037844384856 ) ) ;
#7477 = CYLINDRICAL_SURFACE ( 'NONE', #5052, 8.050000000000000711 ) ;
#7478 = VECTOR ( 'NONE', #13394, 1000.000000000000000 ) ;
#7479 = VERTEX_POINT ( 'NONE', #4290 ) ;
#7480 = CARTESIAN_POINT ( 'NONE',  ( 15.50000000000000000, -5.000000000000000000, 22.50000000000000000 ) ) ;
#7481 = ORIENTED_EDGE ( 'NONE', *, *, #13702, .F. ) ;
#7482 = AXIS2_PLACEMENT_3D ( 'NONE', #1210, #13013, #4550 ) ;
#7483 = ORIENTED_EDGE ( 'NONE', *, *, #725, .T. ) ;
#7484 = ORIENTED_EDGE ( 'NONE', *, *, #2052, .T. ) ;
#7485 = UNCERTAINTY_MEASURE_WITH_UNIT (LENGTH_MEASURE( 1.000000000000000082E-05 ), #8031, 'distance_accuracy_value', 'NONE');
#7486 = FACE_OUTER_BOUND ( 'NONE', #10237, .T. ) ;
#7487 = CARTESIAN_POINT ( 'NONE',  ( -2.834780744084784310, -6.006874999999924469, -1.516137112471814596 ) ) ;
#7488 = CIRCLE ( 'NONE', #771, 10.49999999999999467 ) ;
#7489 = LINE ( 'NONE', #11122, #14033 ) ;
#7490 = CARTESIAN_POINT ( 'NONE',  ( -52.77438362644000591, 65.17411849586700612, -145.4984795835769660 ) ) ;
#7491 = CARTESIAN_POINT ( 'NONE',  ( -69.77438362644001302, 82.17411849586700612, -80.44847958357698303 ) ) ;
#7492 = CIRCLE ( 'NONE', #775, 2.431404194366992400 ) ;
#7493 = DIRECTION ( 'NONE',  ( 0.000000000000000000, -4.336808689942017736E-16, 1.000000000000000000 ) ) ;
#7494 = CARTESIAN_POINT ( 'NONE',  ( -85.77438362644001302, 82.17411849586700612, -138.4984795835769944 ) ) ;
#7495 = CIRCLE ( 'NONE', #779, 2.042000000000002036 ) ;
#7496 = CARTESIAN_POINT ( 'NONE',  ( -3.127990687458614971, 2.260916199238037239E-16, 54.09781049769389938 ) ) ;
#7497 = ORIENTED_EDGE ( 'NONE', *, *, #8487, .F. ) ;
#7498 = DIRECTION ( 'NONE',  ( -2.551930889570660354E-15, 1.000000000000000000, 0.000000000000000000 ) ) ;
#7499 = AXIS2_PLACEMENT_3D ( 'NONE', #10245, #1014, #2183 ) ;
#7500 = ORIENTED_EDGE ( 'NONE', *, *, #15012, .T. ) ;
#7501 = AXIS2_PLACEMENT_3D ( 'NONE', #11346, #1011, #5460 ) ;
#7502 = CARTESIAN_POINT ( 'NONE',  ( -3.144577161339557669, -2.390624999999865885, -2.578777943664209982 ) ) ;
#7503 = EDGE_LOOP ( 'NONE', ( #6080, #1700, #2191 ) ) ;
#7504 = AXIS2_PLACEMENT_3D ( 'NONE', #11372, #739, #10587 ) ;
#7505 = CARTESIAN_POINT ( 'NONE',  ( -3.840936051835830423, -3.530463562373013175, 0.7654668794366149553 ) ) ;
#7506 = DIRECTION ( 'NONE',  ( 1.000000000000000000, 0.000000000000000000, 0.000000000000000000 ) ) ;
#7507 = DIRECTION ( 'NONE',  ( 1.000000000000000000, 0.000000000000000000, 0.000000000000000000 ) ) ;
#7508 = MECHANICAL_DESIGN_GEOMETRIC_PRESENTATION_REPRESENTATION (  '', ( #796 ), #14919 ) ;
#7509 = DIRECTION ( 'NONE',  ( 0.000000000000000000, 0.000000000000000000, 1.000000000000000000 ) ) ;
#7510 = CARTESIAN_POINT ( 'NONE',  ( -83.02438362643998460, 65.17411849586700612, -150.4984795835770228 ) ) ;
#7511 =( GEOMETRIC_REPRESENTATION_CONTEXT ( 3 ) GLOBAL_UNCERTAINTY_ASSIGNED_CONTEXT ( ( #7485 ) ) GLOBAL_UNIT_ASSIGNED_CONTEXT ( ( #8031, #3156, #969 ) ) REPRESENTATION_CONTEXT ( 'NONE', 'WORKASPACE' ) );
#7512 = CARTESIAN_POINT ( 'NONE',  ( -52.77438362644100067, 99.17411849586700612, -79.59847958357700293 ) ) ;
#7513 = FACE_OUTER_BOUND ( 'NONE', #12259, .T. ) ;
#7514 = DIRECTION ( 'NONE',  ( -0.000000000000000000, 1.000000000000000000, -0.000000000000000000 ) ) ;
#7515 = DIRECTION ( 'NONE',  ( -1.000000000000000000, 0.000000000000000000, 0.000000000000000000 ) ) ;
#7516 = VECTOR ( 'NONE', #14615, 1000.000000000000000 ) ;
#7517 = VERTEX_POINT ( 'NONE', #12441 ) ;
#7518 = ORIENTED_EDGE ( 'NONE', *, *, #4284, .F. ) ;
#7519 = EDGE_CURVE ( 'NONE', #3577, #14784, #719, .T. ) ;
#7520 = VERTEX_POINT ( 'NONE', #10028 ) ;
#7521 = CIRCLE ( 'NONE', #10471, 1.999999999999988010 ) ;
#7522 = CARTESIAN_POINT ( 'NONE',  ( -91.27438362643999881, 99.17411849586700612, -86.49847958357699440 ) ) ;
#7523 = CARTESIAN_POINT ( 'NONE',  ( 0.7342756466162191353, -1.803750000000060361, -3.698544502508175569 ) ) ;
#7524 = VERTEX_POINT ( 'NONE', #2979 ) ;
#7525 = ADVANCED_FACE ( 'NONE', ( #3982 ), #563, .F. ) ;
#7526 = LINE ( 'NONE', #8745, #8201 ) ;
#7527 = AXIS2_PLACEMENT_3D ( 'NONE', #2639, #14273, #9679 ) ;
#7528 = CARTESIAN_POINT ( 'NONE',  ( -1.919346139099063597, -5.205827266973400036, -3.000085783918466031 ) ) ;
#7529 = DIRECTION ( 'NONE',  ( 0.000000000000000000, -0.000000000000000000, 1.000000000000000000 ) ) ;
#7530 = AXIS2_PLACEMENT_3D ( 'NONE', #10461, #10544, #10700 ) ;
#7531 = FACE_OUTER_BOUND ( 'NONE', #12236, .T. ) ;
#7532 = SURFACE_SIDE_STYLE ('',( #13269 ) ) ;
#7533 = CARTESIAN_POINT ( 'NONE',  ( -23.25000000000000000, 0.000000000000000000, -27.00000000000000000 ) ) ;
#7534 = DIRECTION ( 'NONE',  ( -1.000000000000000000, -0.000000000000000000, -0.000000000000000000 ) ) ;
#7535 = ORIENTED_EDGE ( 'NONE', *, *, #8184, .T. ) ;
#7536 = CARTESIAN_POINT ( 'NONE',  ( -14.45366306705349757, -0.2717122460102549542, 23.33927276307431242 ) ) ;
#7537 = AXIS2_PLACEMENT_3D ( 'NONE', #12762, #7882, #12614 ) ;
#7538 = EDGE_CURVE ( 'NONE', #10872, #14575, #1664, .T. ) ;
#7539 = AXIS2_PLACEMENT_3D ( 'NONE', #15250, #2226, #15092 ) ;
#7540 = EDGE_LOOP ( 'NONE', ( #1353, #2175 ) ) ;
#7541 = VERTEX_POINT ( 'NONE', #5229 ) ;
#7542 = ORIENTED_EDGE ( 'NONE', *, *, #2125, .T. ) ;
#7543 = ORIENTED_EDGE ( 'NONE', *, *, #3562, .F. ) ;
#7544 = EDGE_CURVE ( 'NONE', #1333, #6631, #6338, .T. ) ;
#7545 = ORIENTED_EDGE ( 'NONE', *, *, #5396, .T. ) ;
#7546 = AXIS2_PLACEMENT_3D ( 'NONE', #10584, #9566, #3685 ) ;
#7547 = DIRECTION ( 'NONE',  ( 0.000000000000000000, 0.000000000000000000, 1.000000000000000000 ) ) ;
#7548 = CARTESIAN_POINT ( 'NONE',  ( 3.722330097189530562, -1.616249999999942899, -0.7418360188101028596 ) ) ;
#7549 = CARTESIAN_POINT ( 'NONE',  ( 2.153747138339810796, -3.843749999999965361, 3.220761568642789729 ) ) ;
#7550 = PLANE ( 'NONE',  #2038 ) ;
#7551 = CIRCLE ( 'NONE', #12244, 16.00000000000000000 ) ;
#7552 = CARTESIAN_POINT ( 'NONE',  ( 16.54686605390242349, -0.2715358723599871626, 21.66103272505201716 ) ) ;
#7553 = EDGE_CURVE ( 'NONE', #7322, #6830, #2906, .T. ) ;
#7554 = DIRECTION ( 'NONE',  ( -1.000000000000000000, 0.000000000000000000, 0.000000000000000000 ) ) ;
#7555 = DIRECTION ( 'NONE',  ( 0.000000000000000000, 1.000000000000000000, 0.000000000000000000 ) ) ;
#7556 = DIRECTION ( 'NONE',  ( 0.000000000000000000, 0.000000000000000000, -1.000000000000000000 ) ) ;
#7557 = DIRECTION ( 'NONE',  ( 0.000000000000000000, 0.000000000000000000, -1.000000000000000000 ) ) ;
#7558 = ORIENTED_EDGE ( 'NONE', *, *, #13592, .F. ) ;
#7559 = DIRECTION ( 'NONE',  ( 0.000000000000000000, 0.000000000000000000, -1.000000000000000000 ) ) ;
#7560 = ADVANCED_FACE ( 'NONE', ( #5165, #9946 ), #2824, .T. ) ;
#7561 = EDGE_LOOP ( 'NONE', ( #6438, #3937, #14579, #3782 ) ) ;
#7562 = VERTEX_POINT ( 'NONE', #13461 ) ;
#7563 = ORIENTED_EDGE ( 'NONE', *, *, #393, .T. ) ;
#7564 = AXIS2_PLACEMENT_3D ( 'NONE', #3818, #6175, #10883 ) ;
#7565 = CIRCLE ( 'NONE', #11508, 17.00000000000000000 ) ;
#7566 = EDGE_CURVE ( 'NONE', #14784, #5278, #1803, .T. ) ;
#7567 = CARTESIAN_POINT ( 'NONE',  ( -35.58670980944424400, 5.000000000000001776, 129.5095611191910621 ) ) ;
#7568 = EDGE_CURVE ( 'NONE', #3958, #9995, #11084, .T. ) ;
#7569 = CARTESIAN_POINT ( 'NONE',  ( 3.252598188045254357, -5.600624999999989306, -0.3215848719029839042 ) ) ;
#7570 = CARTESIAN_POINT ( 'NONE',  ( -6.714472293954754534, 11.99999970914575975, 37.72291661448763733 ) ) ;
#7571 = LINE ( 'NONE', #9943, #4748 ) ;
#7572 = DIRECTION ( 'NONE',  ( 0.000000000000000000, 1.000000000000000000, 0.000000000000000000 ) ) ;
#7573 = ADVANCED_FACE ( 'NONE', ( #11277 ), #8713, .T. ) ;
#7574 = CARTESIAN_POINT ( 'NONE',  ( -69.77438362644001302, 74.17411849586699191, -29.37106258560738681 ) ) ;
#7575 = DIRECTION ( 'NONE',  ( 0.000000000000000000, -1.000000000000000000, 0.000000000000000000 ) ) ;
#7576 = DIRECTION ( 'NONE',  ( 0.000000000000000000, -0.000000000000000000, -1.000000000000000000 ) ) ;
#7577 = ORIENTED_EDGE ( 'NONE', *, *, #5432, .F. ) ;
#7578 = VECTOR ( 'NONE', #12048, 1000.000000000000000 ) ;
#7579 = CARTESIAN_POINT ( 'NONE',  ( -82.27438362643999881, 99.17411849586700612, -145.4984795835769660 ) ) ;
#7580 = EDGE_CURVE ( 'NONE', #15237, #2560, #7791, .T. ) ;
#7581 = ORIENTED_EDGE ( 'NONE', *, *, #8222, .F. ) ;
#7582 = CARTESIAN_POINT ( 'NONE',  ( 3.091873775341146491, -2.890625000000027534, 2.538798244104332191 ) ) ;
#7583 = ORIENTED_EDGE ( 'NONE', *, *, #4711, .F. ) ;
#7584 = AXIS2_PLACEMENT_3D ( 'NONE', #10378, #8425, #13167 ) ;
#7585 = DIRECTION ( 'NONE',  ( 0.000000000000000000, 0.000000000000000000, 1.000000000000000000 ) ) ;
#7586 = FACE_OUTER_BOUND ( 'NONE', #14309, .T. ) ;
#7587 = CARTESIAN_POINT ( 'NONE',  ( -69.77438362644001302, 82.17411849586700612, -51.99847958357699440 ) ) ;
#7588 = CARTESIAN_POINT ( 'NONE',  ( -82.27438362643999881, 65.17411849586700612, -86.49847958357699440 ) ) ;
#7589 = DIRECTION ( 'NONE',  ( 0.000000000000000000, 0.000000000000000000, -1.000000000000000000 ) ) ;
#7590 = CARTESIAN_POINT ( 'NONE',  ( -54.81638362644000040, 63.99516924618178848, -147.9984795835769944 ) ) ;
#7591 = DIRECTION ( 'NONE',  ( 0.000000000000000000, 0.000000000000000000, -1.000000000000000000 ) ) ;
#7592 =( GEOMETRIC_REPRESENTATION_CONTEXT ( 3 ) GLOBAL_UNCERTAINTY_ASSIGNED_CONTEXT ( ( #7785 ) ) GLOBAL_UNIT_ASSIGNED_CONTEXT ( ( #348, #433, #2832 ) ) REPRESENTATION_CONTEXT ( 'NONE', 'WORKASPACE' ) );
#7593 = PLANE ( 'NONE',  #14998 ) ;
#7594 = CARTESIAN_POINT ( 'NONE',  ( 66.41329019055577021, 0.000000000000000000, 89.50956111919107627 ) ) ;
#7595 = AXIS2_PLACEMENT_3D ( 'NONE', #2054, #11520, #4306 ) ;
#7596 = CIRCLE ( 'NONE', #13784, 4.249999999999996447 ) ;
#7597 = ORIENTED_EDGE ( 'NONE', *, *, #13677, .F. ) ;
#7598 = ORIENTED_EDGE ( 'NONE', *, *, #5464, .F. ) ;
#7599 = DIRECTION ( 'NONE',  ( 0.000000000000000000, 0.000000000000000000, -1.000000000000000000 ) ) ;
#7600 = CARTESIAN_POINT ( 'NONE',  ( -2.441443777772109414, -1.225625000000065912, 2.973322847374054501 ) ) ;
#7601 = ORIENTED_EDGE ( 'NONE', *, *, #7566, .F. ) ;
#7602 = VECTOR ( 'NONE', #6842, 1000.000000000000000 ) ;
#7603 = CARTESIAN_POINT ( 'NONE',  ( 23.25000000000000000, 0.000000000000000000, 27.00000000000000000 ) ) ;
#7604 = AXIS2_PLACEMENT_3D ( 'NONE', #8238, #2418, #1100 ) ;
#7605 = AXIS2_PLACEMENT_3D ( 'NONE', #4063, #12207, #1581 ) ;
#7606 = DIRECTION ( 'NONE',  ( -0.4999999999999832356, 0.000000000000000000, 0.8660254037844483666 ) ) ;
#7607 = DIRECTION ( 'NONE',  ( 1.000000000000000000, 0.000000000000000000, 0.000000000000000000 ) ) ;
#7608 = CARTESIAN_POINT ( 'NONE',  ( -0.3198136352484399758, -0.4995676945082599407, -4.144957434285039710 ) ) ;
#7609 = CARTESIAN_POINT ( 'NONE',  ( -69.77438362644001302, 82.17411849586700612, -150.4984795835769944 ) ) ;
#7610 = DIRECTION ( 'NONE',  ( 0.000000000000000000, 1.000000000000000000, 0.000000000000000000 ) ) ;
#7611 = EDGE_CURVE ( 'NONE', #7838, #13165, #1731, .T. ) ;
#7612 = FACE_OUTER_BOUND ( 'NONE', #9748, .T. ) ;
#7613 = ORIENTED_EDGE ( 'NONE', *, *, #8658, .F. ) ;
#7614 = FACE_OUTER_BOUND ( 'NONE', #13076, .T. ) ;
#7615 = ORIENTED_EDGE ( 'NONE', *, *, #5269, .F. ) ;
#7616 = B_SPLINE_CURVE_WITH_KNOTS ( 'NONE', 3,
 ( #1963, #4151, #6712, #4291, #8873, #7792, #2980, #3275 ),
 .UNSPECIFIED., .F., .F.,
 ( 4, 2, 2, 4 ),
 ( 0.04105254269951071067, 0.04300721795512767176, 0.04398455558293615231, 0.04496189321074463285 ),
 .UNSPECIFIED. ) ;
#7617 = VECTOR ( 'NONE', #5989, 1000.000000000000000 ) ;
#7618 = ORIENTED_EDGE ( 'NONE', *, *, #6513, .F. ) ;
#7619 = ORIENTED_EDGE ( 'NONE', *, *, #2337, .T. ) ;
#7620 = ORIENTED_EDGE ( 'NONE', *, *, #7986, .T. ) ;
#7621 = VERTEX_POINT ( 'NONE', #4150 ) ;
#7622 = DIRECTION ( 'NONE',  ( 0.000000000000000000, 1.000000000000000000, 0.000000000000000000 ) ) ;
#7623 = CARTESIAN_POINT ( 'NONE',  ( -3.717546150574369879, -2.069374999999891607, -0.3671215460811757536 ) ) ;
#7624 = LINE ( 'NONE', #13589, #9044 ) ;
#7625 = VECTOR ( 'NONE', #15132, 1000.000000000000114 ) ;
#7626 = PRODUCT_DEFINITION ( 'UNKNOWN', '', #1226, #14753 ) ;
#7627 = CARTESIAN_POINT ( 'NONE',  ( -3.771471614353887336, -4.484375000000117240, -0.3724498170710106582 ) ) ;
#7628 = CARTESIAN_POINT ( 'NONE',  ( -86.77438362644100778, 96.81621999649657084, -147.9984795835769944 ) ) ;
#7629 = EDGE_CURVE ( 'NONE', #10445, #5739, #9874, .T. ) ;
#7630 = DIRECTION ( 'NONE',  ( -1.000000000000000000, 0.000000000000000000, 0.000000000000000000 ) ) ;
#7631 = CIRCLE ( 'NONE', #12817, 10.49999999999999467 ) ;
#7632 = LINE ( 'NONE', #14662, #15294 ) ;
#7633 = CARTESIAN_POINT ( 'NONE',  ( -1.962865815818235271, -1.671875000000012879, 3.669921287786785502 ) ) ;
#7634 = DIRECTION ( 'NONE',  ( 0.000000000000000000, 1.000000000000000000, 0.000000000000000000 ) ) ;
#7635 = LINE ( 'NONE', #1870, #1125 ) ;
#7636 = CARTESIAN_POINT ( 'NONE',  ( -67.13357088346970158, 89.17411849586699191, -44.45439862457462965 ) ) ;
#7637 = ORIENTED_EDGE ( 'NONE', *, *, #3623, .T. ) ;
#7638 = FACE_OUTER_BOUND ( 'NONE', #7350, .T. ) ;
#7639 = EDGE_LOOP ( 'NONE', ( #1046, #11671, #12474, #10939 ) ) ;
#7640 = ORIENTED_EDGE ( 'NONE', *, *, #3009, .T. ) ;
#7641 = EDGE_LOOP ( 'NONE', ( #5410, #1318, #11491, #11755, #5534, #14671 ) ) ;
#7642 = PRODUCT_DEFINITION_CONTEXT ( 'detailed design', #884, 'design' ) ;
#7643 = AXIS2_PLACEMENT_3D ( 'NONE', #4217, #423, #14602 ) ;
#7644 = CARTESIAN_POINT ( 'NONE',  ( -0.9391448502757393513, -5.881874999999767262, -3.091762488354311778 ) ) ;
#7645 = CARTESIAN_POINT ( 'NONE',  ( -52.77438362643999881, 65.17411849586700612, -145.4984795835769944 ) ) ;
#7646 = CARTESIAN_POINT ( 'NONE',  ( 57.41329019055577021, 5.000000000000000000, 99.29549861919106490 ) ) ;
#7647 = EDGE_CURVE ( 'NONE', #2744, #2455, #14307, .T. ) ;
#7648 = CARTESIAN_POINT ( 'NONE',  ( -52.77438362644000591, 99.17411849586700612, -152.4984795835769944 ) ) ;
#7649 = CARTESIAN_POINT ( 'NONE',  ( -86.77438362644100778, 101.5320169952374414, -150.4984795835770228 ) ) ;
#7650 = CARTESIAN_POINT ( 'NONE',  ( 63.41329019055576310, 5.000000000000000000, 137.5095611191910621 ) ) ;
#7651 = EDGE_CURVE ( 'NONE', #6323, #8857, #1926, .T. ) ;
#7652 = CIRCLE ( 'NONE', #14569, 4.000000000000000888 ) ;
#7653 = CARTESIAN_POINT ( 'NONE',  ( 21.98164641901421135, -11.40000029085424238, -0.3335879563140091153 ) ) ;
#7654 = ADVANCED_FACE ( 'NONE', ( #11353 ), #11193, .F. ) ;
#7655 = ORIENTED_EDGE ( 'NONE', *, *, #490, .T. ) ;
#7656 = FACE_OUTER_BOUND ( 'NONE', #11572, .T. ) ;
#7657 = ITEM_DEFINED_TRANSFORMATION ( 'NONE', 'NONE', #12452,  #285 ) ;
#7658 = ORIENTED_EDGE ( 'NONE', *, *, #1086, .T. ) ;
#7659 = DIRECTION ( 'NONE',  ( 1.000000000000000000, 0.000000000000000000, 0.000000000000000000 ) ) ;
#7660 = EDGE_CURVE ( 'NONE', #5822, #13943, #7394, .T. ) ;
#7661 = CARTESIAN_POINT ( 'NONE',  ( 0.3862366009532263167, -3.234374999999897859, -3.936230821419137271 ) ) ;
#7662 = ORIENTED_EDGE ( 'NONE', *, *, #3510, .F. ) ;
#7663 = CIRCLE ( 'NONE', #9372, 1.785937500000001066 ) ;
#7664 = CARTESIAN_POINT ( 'NONE',  ( -54.81638362644000040, 63.99516924618178848, -147.9984795835769944 ) ) ;
#7665 = EDGE_CURVE ( 'NONE', #6231, #9550, #11501, .T. ) ;
#7666 = CARTESIAN_POINT ( 'NONE',  ( 15.50000000000000000, -2.500000000000000000, -23.94337567297399971 ) ) ;
#7667 = CARTESIAN_POINT ( 'NONE',  ( -61.64938362644000591, 82.17411849586700612, -79.49847958357700861 ) ) ;
#7668 = EDGE_CURVE ( 'NONE', #5306, #7524, #3351, .T. ) ;
#7669 = CARTESIAN_POINT ( 'NONE',  ( -69.77438362644001302, 82.17411849586700612, -117.9984795835769944 ) ) ;
#7670 = PLANE ( 'NONE',  #4866 ) ;
#7671 = CARTESIAN_POINT ( 'NONE',  ( -67.81379359564340348, 98.05581852273024879, -94.29007922354536220 ) ) ;
#7672 = AXIS2_PLACEMENT_3D ( 'NONE', #1747, #6497, #8505 ) ;
#7673 = ORIENTED_EDGE ( 'NONE', *, *, #393, .F. ) ;
#7674 = EDGE_LOOP ( 'NONE', ( #9992, #11267 ) ) ;
#7675 = DIRECTION ( 'NONE',  ( -1.000000000000000000, 0.000000000000000000, 0.000000000000000000 ) ) ;
#7676 = CARTESIAN_POINT ( 'NONE',  ( -3.865847815970003598, -1.085000000000063469, -0.001011349278449839070 ) ) ;
#7677 = ORIENTED_EDGE ( 'NONE', *, *, #13873, .F. ) ;
#7678 = CARTESIAN_POINT ( 'NONE',  ( -86.77438362644100778, 99.17411849586700612, -79.59847958357700293 ) ) ;
#7679 = CARTESIAN_POINT ( 'NONE',  ( -3.466497813382189541, -5.275048774667015827, -7.182839392716466875E-16 ) ) ;
#7680 = CARTESIAN_POINT ( 'NONE',  ( 3.031088913245533423, 0.04639863247564009890, -3.749999999999999556 ) ) ;
#7681 = DIRECTION ( 'NONE',  ( 0.000000000000000000, 0.000000000000000000, 1.000000000000000000 ) ) ;
#7682 = FACE_OUTER_BOUND ( 'NONE', #10408, .T. ) ;
#7683 = CARTESIAN_POINT ( 'NONE',  ( 22.58164641901420921, 3.685382519066023654, 0.01788390626213402432 ) ) ;
#7684 = FACE_OUTER_BOUND ( 'NONE', #10520, .T. ) ;
#7685 = ORIENTED_EDGE ( 'NONE', *, *, #5839, .F. ) ;
#7686 = DIRECTION ( 'NONE',  ( 0.000000000000000000, 1.000000000000000000, 0.000000000000000000 ) ) ;
#7687 = ORIENTED_EDGE ( 'NONE', *, *, #3062, .F. ) ;
#7688 = ORIENTED_EDGE ( 'NONE', *, *, #14820, .T. ) ;
#7689 = ORIENTED_EDGE ( 'NONE', *, *, #14731, .T. ) ;
#7690 = EDGE_LOOP ( 'NONE', ( #11628, #1797, #6226, #3240 ) ) ;
#7691 = ORIENTED_EDGE ( 'NONE', *, *, #3458, .T. ) ;
#7692 =( BOUNDED_CURVE ( )  B_SPLINE_CURVE ( 3, ( #12822, #12599, #14977, #13834 ),
 .UNSPECIFIED., .F., .T. ) 
 B_SPLINE_CURVE_WITH_KNOTS ( ( 4, 4 ),
 ( 5.777824796895650650, 6.283185307179590673 ),
 .UNSPECIFIED. ) 
 CURVE ( )  GEOMETRIC_REPRESENTATION_ITEM ( )  RATIONAL_B_SPLINE_CURVE ( ( 1.000000000000000000, 0.9788305577012550440, 0.9788305577012550440, 1.000000000000000000 ) ) 
 REPRESENTATION_ITEM ( '' )  );
#7693 = DIRECTION ( 'NONE',  ( -0.08715574274766166307, -4.420346012544052123E-16, 0.9961946980917453232 ) ) ;
#7694 = ADVANCED_FACE ( 'NONE', ( #11734 ), #3130, .F. ) ;
#7695 = SURFACE_STYLE_USAGE ( .BOTH. , #15033 ) ;
#7696 = CARTESIAN_POINT ( 'NONE',  ( -0.3756913567350075311, -4.265625000000119904, -3.800190021185207545 ) ) ;
#7697 = FACE_OUTER_BOUND ( 'NONE', #7561, .T. ) ;
#7698 = LINE ( 'NONE', #10079, #1906 ) ;
#7699 = CARTESIAN_POINT ( 'NONE',  ( -54.81638362644000040, 63.99516924618178848, -147.9984795835769944 ) ) ;
#7700 = CARTESIAN_POINT ( 'NONE',  ( 2.374332146000840194, -0.8437500000000230926, 3.550666350934340354 ) ) ;
#7701 = DIRECTION ( 'NONE',  ( 1.000000000000000000, 0.000000000000000000, 0.000000000000000000 ) ) ;
#7702 = PRODUCT_DEFINITION_SHAPE ( 'NONE', 'NONE',  #7428 ) ;
#7703 = DIRECTION ( 'NONE',  ( -1.287488025362404182E-15, -1.000000000000000000, 0.000000000000000000 ) ) ;
#7704 = ORIENTED_EDGE ( 'NONE', *, *, #7448, .T. ) ;
#7705 = LINE ( 'NONE', #11406, #6293 ) ;
#7706 = ORIENTED_EDGE ( 'NONE', *, *, #1560, .F. ) ;
#7707 = ORIENTED_EDGE ( 'NONE', *, *, #12108, .F. ) ;
#7708 = ORIENTED_EDGE ( 'NONE', *, *, #9609, .T. ) ;
#7709 = EDGE_CURVE ( 'NONE', #8931, #2834, #7008, .T. ) ;
#7710 = LINE ( 'NONE', #2735, #2763 ) ;
#7711 = CARTESIAN_POINT ( 'NONE',  ( -2.276987973263394416, -5.960000000000099440, -2.278132229539954867 ) ) ;
#7712 = EDGE_CURVE ( 'NONE', #12468, #7562, #15286, .T. ) ;
#7713 = CARTESIAN_POINT ( 'NONE',  ( -96.77438362643999881, 59.67411849586700612, -152.4984795835769944 ) ) ;
#7714 = DIRECTION ( 'NONE',  ( -1.747085166004344019E-15, 1.000000000000000000, -0.000000000000000000 ) ) ;
#7715 = DIRECTION ( 'NONE',  ( 1.000000000000000000, 0.000000000000000000, 0.000000000000000000 ) ) ;
#7716 = DIRECTION ( 'NONE',  ( 1.287488025362404182E-15, 1.000000000000000000, 0.000000000000000000 ) ) ;
#7717 = CARTESIAN_POINT ( 'NONE',  ( -38.27438362644000591, 60.67411849586700612, -67.49847958357700861 ) ) ;
#7718 = DIRECTION ( 'NONE',  ( 1.000000000000000000, -0.000000000000000000, 0.000000000000000000 ) ) ;
#7719 = ORIENTED_EDGE ( 'NONE', *, *, #5074, .T. ) ;
#7720 = PLANE ( 'NONE',  #12327 ) ;
#7721 = EDGE_CURVE ( 'NONE', #4925, #3944, #186, .T. ) ;
#7722 = ORIENTED_EDGE ( 'NONE', *, *, #11429, .T. ) ;
#7723 = AXIS2_PLACEMENT_3D ( 'NONE', #5243, #4162, #575 ) ;
#7724 = FACE_OUTER_BOUND ( 'NONE', #3723, .T. ) ;
#7725 = CARTESIAN_POINT ( 'NONE',  ( 3.946741062051739579, -1.953124999999941380, 1.198372487375103157 ) ) ;
#7726 = ORIENTED_EDGE ( 'NONE', *, *, #13327, .F. ) ;
#7727 = EDGE_CURVE ( 'NONE', #51, #10402, #11345, .T. ) ;
#7728 = CIRCLE ( 'NONE', #6260, 4.000000000000000888 ) ;
#7729 = DIRECTION ( 'NONE',  ( 0.000000000000000000, 0.000000000000000000, -1.000000000000000000 ) ) ;
#7730 = FACE_OUTER_BOUND ( 'NONE', #6166, .T. ) ;
#7731 = AXIS2_PLACEMENT_3D ( 'NONE', #6028, #8482, #7334 ) ;
#7732 = ADVANCED_FACE ( 'NONE', ( #4681 ), #10336, .F. ) ;
#7733 = CARTESIAN_POINT ( 'NONE',  ( -4.522482571421200248, 10.99999970914572422, 70.03692566716178192 ) ) ;
#7734 = CARTESIAN_POINT ( 'NONE',  ( -0.4546285098678428671, 2.357490090293554275, 4.500000000000001776 ) ) ;
#7735 = ADVANCED_FACE ( 'NONE', ( #1101 ), #1962, .F. ) ;
#7736 = DIRECTION ( 'NONE',  ( 0.000000000000000000, 0.000000000000000000, -1.000000000000000000 ) ) ;
#7737 = DIRECTION ( 'NONE',  ( 0.000000000000000000, 0.000000000000000000, 1.000000000000000000 ) ) ;
#7738 = CARTESIAN_POINT ( 'NONE',  ( -52.77438362643999881, 65.17411849586700612, -145.4984795835769944 ) ) ;
#7739 = VERTEX_POINT ( 'NONE', #4370 ) ;
#7740 = CIRCLE ( 'NONE', #5255, 2.700000000000001066 ) ;
#7741 = ADVANCED_FACE ( 'NONE', ( #3274 ), #10399, .F. ) ;
#7742 = VERTEX_POINT ( 'NONE', #11650 ) ;
#7743 =( REPRESENTATION_RELATIONSHIP ('NONE','NONE', #12357, #6613 ) REPRESENTATION_RELATIONSHIP_WITH_TRANSFORMATION ( #5478 )SHAPE_REPRESENTATION_RELATIONSHIP( ) );
#7744 = FACE_OUTER_BOUND ( 'NONE', #4452, .T. ) ;
#7745 = CARTESIAN_POINT ( 'NONE',  ( -2.746234728672138026, -0.9599999999999920819, -2.744228674164193471 ) ) ;
#7746 = ORIENTED_EDGE ( 'NONE', *, *, #53, .F. ) ;
#7747 = EDGE_CURVE ( 'NONE', #10998, #7389, #2110, .T. ) ;
#7748 = AXIS2_PLACEMENT_3D ( 'NONE', #9219, #1077, #10620 ) ;
#7749 = EDGE_CURVE ( 'NONE', #3577, #8760, #5546, .T. ) ;
#7750 = DIRECTION ( 'NONE',  ( 0.000000000000000000, 0.000000000000000000, -1.000000000000000000 ) ) ;
#7751 = DIRECTION ( 'NONE',  ( 1.000000000000000000, 0.000000000000000000, 0.000000000000000000 ) ) ;
#7752 = TOROIDAL_SURFACE ( 'NONE', #10708, 2.700000000000000178, 0.2000000000000000111 ) ;
#7753 = CARTESIAN_POINT ( 'NONE',  ( -0.8000000000000104805, 8.384405323238834029, 0.000000000000000000 ) ) ;
#7754 = CARTESIAN_POINT ( 'NONE',  ( 4.573385150445044900, -19.31989681812820692, 6.000000000000001776 ) ) ;
#7755 = FILL_AREA_STYLE ('',( #9910 ) ) ;
#7756 = LINE ( 'NONE', #680, #634 ) ;
#7757 = DIRECTION ( 'NONE',  ( -0.8660254037844485886, 0.000000000000000000, -0.4999999999999827360 ) ) ;
#7758 = VECTOR ( 'NONE', #828, 1000.000000000000000 ) ;
#7759 = ORIENTED_EDGE ( 'NONE', *, *, #14404, .F. ) ;
#7760 = CARTESIAN_POINT ( 'NONE',  ( -15.50000000000000000, -0.4000000000000000222, 22.50000000000000000 ) ) ;
#7761 = EDGE_CURVE ( 'NONE', #6139, #3708, #7692, .T. ) ;
#7762 = ORIENTED_EDGE ( 'NONE', *, *, #4485, .T. ) ;
#7763 = VERTEX_POINT ( 'NONE', #10248 ) ;
#7764 = ORIENTED_EDGE ( 'NONE', *, *, #1354, .T. ) ;
#7765 = EDGE_LOOP ( 'NONE', ( #12070, #7445, #7620, #631, #8509, #10215, #10292, #6383, #13115, #11692 ) ) ;
#7766 = VECTOR ( 'NONE', #10005, 1000.000000000000000 ) ;
#7767 = VERTEX_POINT ( 'NONE', #14061 ) ;
#7768 = CARTESIAN_POINT ( 'NONE',  ( -3.581950731666862175, -5.530463562373103770, 0.7115315330189105891 ) ) ;
#7769 = CARTESIAN_POINT ( 'NONE',  ( -0.001042462806609206153, -0.3350000000001150946, 3.965061882346304412 ) ) ;
#7770 = LINE ( 'NONE', #11477, #3851 ) ;
#7771 = CARTESIAN_POINT ( 'NONE',  ( 4.096389842826703820, -2.015625000000050182, -0.4049582849837481402 ) ) ;
#7772 = CARTESIAN_POINT ( 'NONE',  ( 15.50000000000000000, 0.000000000000000000, 26.50000000000000000 ) ) ;
#7773 = FACE_OUTER_BOUND ( 'NONE', #5441, .T. ) ;
#7774 = LINE ( 'NONE', #11258, #13339 ) ;
#7775 = CARTESIAN_POINT ( 'NONE',  ( 3.275404563695782034, -1.109375000000065503, -2.686596450795923463 ) ) ;
#7776 = CARTESIAN_POINT ( 'NONE',  ( -89.47438362643998744, 65.17411849586700612, -145.2984795835770058 ) ) ;
#7777 = CARTESIAN_POINT ( 'NONE',  ( 15.50000000000000000, -0.4000000000005274892, -19.20000000000052864 ) ) ;
#7778 = VECTOR ( 'NONE', #2966, 1000.000000000000000 ) ;
#7779 = DIRECTION ( 'NONE',  ( -1.000000000000000000, 0.000000000000000000, 0.000000000000000000 ) ) ;
#7780 = ORIENTED_EDGE ( 'NONE', *, *, #8692, .F. ) ;
#7781 = DIRECTION ( 'NONE',  ( 0.000000000000000000, 1.000000000000000000, 0.000000000000000000 ) ) ;
#7782 = ORIENTED_EDGE ( 'NONE', *, *, #8922, .F. ) ;
#7783 = EDGE_LOOP ( 'NONE', ( #12156, #10996, #5998, #2043, #13604, #2638 ) ) ;
#7784 = ORIENTED_EDGE ( 'NONE', *, *, #2147, .T. ) ;
#7785 = UNCERTAINTY_MEASURE_WITH_UNIT (LENGTH_MEASURE( 1.000000000000000082E-05 ), #348, 'distance_accuracy_value', 'NONE');
#7786 = CARTESIAN_POINT ( 'NONE',  ( -6.714472293954755422, -12.00000029085427578, 37.72291661448763733 ) ) ;
#7787 = AXIS2_PLACEMENT_3D ( 'NONE', #6826, #13941, #3315 ) ;
#7788 = FACE_OUTER_BOUND ( 'NONE', #13453, .T. ) ;
#7789 = DIRECTION ( 'NONE',  ( 0.000000000000000000, 0.000000000000000000, 1.000000000000000000 ) ) ;
#7790 = DIRECTION ( 'NONE',  ( -1.000000000000000000, 0.000000000000000000, 0.000000000000000000 ) ) ;
#7791 = LINE ( 'NONE', #7649, #1672 ) ;
#7792 = CARTESIAN_POINT ( 'NONE',  ( -70.45539183192724408, 75.17411849586700612, -44.02377680093038492 ) ) ;
#7793 = EDGE_CURVE ( 'NONE', #3281, #10624, #3913, .T. ) ;
#7794 = FACE_OUTER_BOUND ( 'NONE', #10423, .T. ) ;
#7795 = EDGE_LOOP ( 'NONE', ( #5173, #5152, #4957, #13891, #1568, #14773 ) ) ;
#7796 = CARTESIAN_POINT ( 'NONE',  ( 2.937061643673781752, -5.103115294876279684, -2.234448363260541193 ) ) ;
#7797 = AXIS2_PLACEMENT_3D ( 'NONE', #13027, #6058, #7209 ) ;
#7798 = AXIS2_PLACEMENT_3D ( 'NONE', #2545, #9668, #9371 ) ;
#7799 = ADVANCED_FACE ( 'NONE', ( #3429 ), #13579, .F. ) ;
#7800 = AXIS2_PLACEMENT_3D ( 'NONE', #7287, #1143, #12091 ) ;
#7801 = EDGE_LOOP ( 'NONE', ( #9264, #6000, #7581, #6440 ) ) ;
#7802 = VERTEX_POINT ( 'NONE', #1018 ) ;
#7803 = CARTESIAN_POINT ( 'NONE',  ( -0.7718104722664602679, -3.281249999999995115, -3.872775259196827857 ) ) ;
#7804 = ORIENTED_EDGE ( 'NONE', *, *, #1640, .F. ) ;
#7805 = LINE ( 'NONE', #8808, #13902 ) ;
#7806 = AXIS2_PLACEMENT_3D ( 'NONE', #3539, #9276, #11767 ) ;
#7807 = FACE_OUTER_BOUND ( 'NONE', #228, .T. ) ;
#7808 = SPHERICAL_SURFACE ( 'NONE', #822, 1.000000000000000000 ) ;
#7809 = ADVANCED_FACE ( 'NONE', ( #12894 ), #2259, .F. ) ;
#7810 = CARTESIAN_POINT ( 'NONE',  ( -3.173335668876506421, -5.500000000000010658, 0.000000000000000000 ) ) ;
#7811 = CARTESIAN_POINT ( 'NONE',  ( 4.573385150445044900, -19.31989681812820692, 6.000000000000001776 ) ) ;
#7812 = DIRECTION ( 'NONE',  ( 1.000000000000000000, 0.000000000000000000, 0.000000000000000000 ) ) ;
#7813 = CARTESIAN_POINT ( 'NONE',  ( 17.21626540049105358, 10.99999970914576330, -12.20299797093197647 ) ) ;
#7814 = EDGE_LOOP ( 'NONE', ( #12239, #5094, #3278, #2557 ) ) ;
#7815 = AXIS2_PLACEMENT_3D ( 'NONE', #508, #9733, #577 ) ;
#7816 = DIRECTION ( 'NONE',  ( 0.8660254037844383745, -0.5000000000000003331, 0.000000000000000000 ) ) ;
#7817 = CARTESIAN_POINT ( 'NONE',  ( 3.779448512589508979, -1.600625000000089226, -0.3712484392070567463 ) ) ;
#7818 = ORIENTED_EDGE ( 'NONE', *, *, #7075, .F. ) ;
#7819 = CIRCLE ( 'NONE', #12763, 1.785937500000001066 ) ;
#7820 = EDGE_CURVE ( 'NONE', #9398, #6550, #5061, .T. ) ;
#7821 = CARTESIAN_POINT ( 'NONE',  ( 33.35543536254877495, -19.31989681812820692, 6.000000000000000000 ) ) ;
#7822 = VECTOR ( 'NONE', #6268, 1000.000000000000000 ) ;
#7823 = AXIS2_PLACEMENT_3D ( 'NONE', #11049, #5001, #3837 ) ;
#7824 = CARTESIAN_POINT ( 'NONE',  ( -52.77438362644000591, 65.17411849586700612, -86.49847958357699440 ) ) ;
#7825 =( LENGTH_UNIT ( ) NAMED_UNIT ( * ) SI_UNIT ( .MILLI., .METRE. ) );
#7826 = AXIS2_PLACEMENT_3D ( 'NONE', #147, #4899, #1078 ) ;
#7827 = CYLINDRICAL_SURFACE ( 'NONE', #10277, 4.000000000000000000 ) ;
#7828 = EDGE_CURVE ( 'NONE', #8472, #11860, #14068, .T. ) ;
#7829 = DIRECTION ( 'NONE',  ( 0.4999999999999827360, 0.000000000000000000, -0.8660254037844485886 ) ) ;
#7830 = EDGE_CURVE ( 'NONE', #3116, #7520, #14890, .T. ) ;
#7831 = ORIENTED_EDGE ( 'NONE', *, *, #416, .F. ) ;
#7832 = DIRECTION ( 'NONE',  ( 0.000000000000000000, 0.000000000000000000, 1.000000000000000000 ) ) ;
#7833 = EDGE_LOOP ( 'NONE', ( #11775, #14818 ) ) ;
#7834 = ORIENTED_EDGE ( 'NONE', *, *, #2795, .F. ) ;
#7835 = VERTEX_POINT ( 'NONE', #13289 ) ;
#7836 = VECTOR ( 'NONE', #4130, 1000.000000000000000 ) ;
#7837 = EDGE_LOOP ( 'NONE', ( #5320, #9209, #1832, #1545 ) ) ;
#7838 = VERTEX_POINT ( 'NONE', #3666 ) ;
#7839 = AXIS2_PLACEMENT_3D ( 'NONE', #5935, #4833, #11648 ) ;
#7840 = FACE_OUTER_BOUND ( 'NONE', #5508, .T. ) ;
#7841 = ADVANCED_FACE ( 'NONE', ( #4834 ), #14559, .T. ) ;
#7842 = VECTOR ( 'NONE', #8481, 1000.000000000000114 ) ;
#7843 = DIRECTION ( 'NONE',  ( 1.000000000000000000, 0.000000000000000000, 0.000000000000000000 ) ) ;
#7844 = CARTESIAN_POINT ( 'NONE',  ( 2.807699568699258297, -3.124999999999853895, -2.806223270957961091 ) ) ;
#7845 = CYLINDRICAL_SURFACE ( 'NONE', #12969, 0.8000000000000113687 ) ;
#7846 = ADVANCED_FACE ( 'NONE', ( #14129 ), #9623, .F. ) ;
#7847 = DIRECTION ( 'NONE',  ( 0.000000000000000000, 0.000000000000000000, 1.000000000000000000 ) ) ;
#7848 = CARTESIAN_POINT ( 'NONE',  ( 3.008642795497740607, 2.054436331234742230, 3.788877816371843288 ) ) ;
#7849 = CARTESIAN_POINT ( 'NONE',  ( -3.245221319803801130, -1.390624999999827915, -2.664727821046819489 ) ) ;
#7850 = AXIS2_PLACEMENT_3D ( 'NONE', #9823, #3486, #5023 ) ;
#7851 = DIRECTION ( 'NONE',  ( 1.224646799147351975E-16, 1.000000000000000000, 0.000000000000000000 ) ) ;
#7852 = DIRECTION ( 'NONE',  ( -0.000000000000000000, 1.000000000000000000, -0.000000000000000000 ) ) ;
#7853 = DIRECTION ( 'NONE',  ( 0.000000000000000000, 1.000000000000000000, 0.000000000000000000 ) ) ;
#7854 = ORIENTED_EDGE ( 'NONE', *, *, #2143, .T. ) ;
#7855 = DIRECTION ( 'NONE',  ( -6.982962677686266711E-15, -6.579622859988665673E-30, -1.000000000000000000 ) ) ;
#7856 = ORIENTED_EDGE ( 'NONE', *, *, #4778, .T. ) ;
#7857 = ORIENTED_EDGE ( 'NONE', *, *, #6506, .F. ) ;
#7858 = EDGE_LOOP ( 'NONE', ( #14312, #10370 ) ) ;
#7859 = CARTESIAN_POINT ( 'NONE',  ( 16.75000000000000000, -2.500000000000000000, 23.22168783648699986 ) ) ;
#7860 = AXIS2_PLACEMENT_3D ( 'NONE', #11447, #7737, #14852 ) ;
#7861 = AXIS2_PLACEMENT_3D ( 'NONE', #9523, #14038, #11635 ) ;
#7862 = CARTESIAN_POINT ( 'NONE',  ( -38.27438362644000591, 111.1741184958670061, -67.49847958357700861 ) ) ;
#7863 = DIRECTION ( 'NONE',  ( -1.000000000000000000, 0.000000000000000000, 0.000000000000000000 ) ) ;
#7864 = DIRECTION ( 'NONE',  ( 0.000000000000000000, 1.000000000000000000, 0.000000000000000000 ) ) ;
#7865 = CARTESIAN_POINT ( 'NONE',  ( -52.77438362644100067, 101.5320169952374414, -147.9984795835769944 ) ) ;
#7866 = DIRECTION ( 'NONE',  ( 0.000000000000000000, 0.000000000000000000, 1.000000000000000000 ) ) ;
#7867 = CARTESIAN_POINT ( 'NONE',  ( -13.41835358098578723, -12.00000029085423137, -56.77834603255778489 ) ) ;
#7868 = CARTESIAN_POINT ( 'NONE',  ( -1.266249875242109413, -5.272499999999733511, 3.060236832100306614 ) ) ;
#7869 = ORIENTED_EDGE ( 'NONE', *, *, #12101, .T. ) ;
#7870 = LINE ( 'NONE', #4072, #13063 ) ;
#7871 = EDGE_LOOP ( 'NONE', ( #14480, #10108, #612 ) ) ;
#7872 = CONICAL_SURFACE ( 'NONE', #4648, 2.042000000000002036, 1.047197551196596965 ) ;
#7873 = CARTESIAN_POINT ( 'NONE',  ( 16.12213235744115636, -12.00000029085424202, 0.3029999373072352897 ) ) ;
#7874 = ORIENTED_EDGE ( 'NONE', *, *, #10334, .T. ) ;
#7875 = CARTESIAN_POINT ( 'NONE',  ( -0.4212280308283230523, -0.7343750000000048850, 4.265137983724988757 ) ) ;
#7876 = ORIENTED_EDGE ( 'NONE', *, *, #14799, .T. ) ;
#7877 = CARTESIAN_POINT ( 'NONE',  ( -2.584068721321989948, -2.358588562373262754, -3.146367359111198247 ) ) ;
#7878 = DIRECTION ( 'NONE',  ( -1.000000000000000000, 0.000000000000000000, 0.000000000000000000 ) ) ;
#7879 = EDGE_CURVE ( 'NONE', #4260, #6663, #7399, .T. ) ;
#7880 = DIRECTION ( 'NONE',  ( -1.000000000000000000, 0.000000000000000000, 0.000000000000000000 ) ) ;
#7881 = AXIS2_PLACEMENT_3D ( 'NONE', #4445, #13903, #2488 ) ;
#7882 = DIRECTION ( 'NONE',  ( -1.000000000000000000, 0.000000000000000000, -0.000000000000000000 ) ) ;
#7883 = CARTESIAN_POINT ( 'NONE',  ( -50.27438362644100067, 59.67411849586700612, -79.59847958357700293 ) ) ;
#7884 = CARTESIAN_POINT ( 'NONE',  ( -15.50000000000000000, 0.000000000000000000, 26.50000000000000000 ) ) ;
#7885 = CARTESIAN_POINT ( 'NONE',  ( 21.98164641901421135, 11.39999970914575833, 0.2664120436859911956 ) ) ;
#7886 = DIRECTION ( 'NONE',  ( -0.08715574274766174634, -4.320305823558445294E-16, 0.9961946980917452121 ) ) ;
#7887 = ORIENTED_EDGE ( 'NONE', *, *, #12089, .F. ) ;
#7888 = AXIS2_PLACEMENT_3D ( 'NONE', #2883, #14739, #4125 ) ;
#7889 = CARTESIAN_POINT ( 'NONE',  ( 3.258191480560295616, -0.6787499999999294653, -2.178773987163739267 ) ) ;
#7890 = ORIENTED_EDGE ( 'NONE', *, *, #10730, .F. ) ;
#7891 = EDGE_CURVE ( 'NONE', #7923, #6403, #7146, .T. ) ;
#7892 = PLANE ( 'NONE',  #3005 ) ;
#7893 = EDGE_CURVE ( 'NONE', #160, #6471, #1416, .T. ) ;
#7894 = CARTESIAN_POINT ( 'NONE',  ( -14.25000000000000000, -0.2038245569916330158, 21.77831216351300014 ) ) ;
#7895 = CIRCLE ( 'NONE', #9616, 4.500000000000003553 ) ;
#7896 = CARTESIAN_POINT ( 'NONE',  ( 3.867986884670384207, -0.4995676945082496712, 0.8486844468283908371 ) ) ;
#7897 = CARTESIAN_POINT ( 'NONE',  ( -15.50000000000000000, -0.2000000000000000111, -22.50000000000000000 ) ) ;
#7898 = CARTESIAN_POINT ( 'NONE',  ( -69.77438362644001302, 82.17411849586700612, -3.496191900462991775 ) ) ;
#7899 = ORIENTED_EDGE ( 'NONE', *, *, #9155, .F. ) ;
#7900 = CARTESIAN_POINT ( 'NONE',  ( -16.75000000000000000, -2.500000000000000000, -23.22168783648699986 ) ) ;
#7901 = VERTEX_POINT ( 'NONE', #14290 ) ;
#7902 = ORIENTED_EDGE ( 'NONE', *, *, #3372, .T. ) ;
#7903 = ORIENTED_EDGE ( 'NONE', *, *, #2505, .F. ) ;
#7904 = ORIENTED_EDGE ( 'NONE', *, *, #12718, .F. ) ;
#7905 = ADVANCED_FACE ( 'NONE', ( #3733 ), #7317, .F. ) ;
#7906 = EDGE_LOOP ( 'NONE', ( #10925, #9203, #7558, #11151 ) ) ;
#7907 = CARTESIAN_POINT ( 'NONE',  ( 3.308479819675366862, -6.061713562373198805, -1.371850503680594802 ) ) ;
#7908 = ADVANCED_FACE ( 'NONE', ( #14430 ), #6174, .F. ) ;
#7909 = FACE_BOUND ( 'NONE', #14396, .T. ) ;
#7910 = CARTESIAN_POINT ( 'NONE',  ( 3.689984836354881281, -2.937500000000126565, 1.529580092797385715 ) ) ;
#7911 = CARTESIAN_POINT ( 'NONE',  ( 15.50000000000000000, -1.037157890325000054, 18.50000000000000000 ) ) ;
#7912 = CARTESIAN_POINT ( 'NONE',  ( -86.77438362643999881, 65.17411849586700612, -145.2984795835770058 ) ) ;
#7913 = DIRECTION ( 'NONE',  ( 0.000000000000000000, 0.000000000000000000, 1.000000000000000000 ) ) ;
#7914 = CARTESIAN_POINT ( 'NONE',  ( -4.184567129761759929, -1.500000000000142109, 0.001513272625389735625 ) ) ;
#7915 = DIRECTION ( 'NONE',  ( -1.000000000000000000, 0.000000000000000000, 0.000000000000000000 ) ) ;
#7916 = CARTESIAN_POINT ( 'NONE',  ( 15.91242688423647600, -0.3152598339557935447, -21.29473909966096556 ) ) ;
#7917 = DIRECTION ( 'NONE',  ( 0.000000000000000000, 0.000000000000000000, 1.000000000000000000 ) ) ;
#7918 = ADVANCED_FACE ( 'NONE', ( #6240 ), #10848, .T. ) ;
#7919 = VERTEX_POINT ( 'NONE', #2342 ) ;
#7920 = FACE_OUTER_BOUND ( 'NONE', #2558, .T. ) ;
#7921 = ORIENTED_EDGE ( 'NONE', *, *, #14987, .T. ) ;
#7922 = EDGE_LOOP ( 'NONE', ( #3870, #14969, #12923, #1929 ) ) ;
#7923 = VERTEX_POINT ( 'NONE', #11813 ) ;
#7924 = PRODUCT_DEFINITION_CONTEXT ( 'detailed design', #5667, 'design' ) ;
#7925 = EDGE_CURVE ( 'NONE', #3798, #9085, #12829, .T. ) ;
#7926 = DIRECTION ( 'NONE',  ( 1.000000000000000000, 0.000000000000000000, 0.000000000000000000 ) ) ;
#7927 = CARTESIAN_POINT ( 'NONE',  ( -3.313940955170693758, -4.131874999999921805, 1.004348227522835924 ) ) ;
#7928 = EDGE_CURVE ( 'NONE', #13728, #5260, #13209, .T. ) ;
#7929 = EDGE_CURVE ( 'NONE', #11895, #13653, #9099, .T. ) ;
#7930 = CARTESIAN_POINT ( 'NONE',  ( 4.763139720814411504, 0.04639863247564429694, 0.7499999999999985567 ) ) ;
#7931 = DIRECTION ( 'NONE',  ( 0.000000000000000000, 0.000000000000000000, 1.000000000000000000 ) ) ;
#7932 = DIRECTION ( 'NONE',  ( 0.000000000000000000, 0.000000000000000000, -1.000000000000000000 ) ) ;
#7933 = DIRECTION ( 'NONE',  ( 0.000000000000000000, 0.000000000000000000, 1.000000000000000000 ) ) ;
#7934 = CARTESIAN_POINT ( 'NONE',  ( 1.624300153006762448, -0.4995676945082549447, 3.676067300042933805 ) ) ;
#7935 = CARTESIAN_POINT ( 'NONE',  ( -64.35475059718073965, 66.06115545897766594, -81.84847958357698872 ) ) ;
#7936 = VERTEX_POINT ( 'NONE', #238 ) ;
#7937 = CARTESIAN_POINT ( 'NONE',  ( 2.931584255716234821, -5.103127331515293186, -2.242088070657691556 ) ) ;
#7938 = ORIENTED_EDGE ( 'NONE', *, *, #12401, .T. ) ;
#7939 = CARTESIAN_POINT ( 'NONE',  ( 68.41329019055577021, 5.000000000000000000, 137.5095611191910621 ) ) ;
#7940 = VERTEX_POINT ( 'NONE', #5936 ) ;
#7941 = CARTESIAN_POINT ( 'NONE',  ( -4.316892141304113473, -0.5000000000000647260, -0.001152797426451617618 ) ) ;
#7942 = ORIENTED_EDGE ( 'NONE', *, *, #10258, .T. ) ;
#7943 = CARTESIAN_POINT ( 'NONE',  ( -3.872011465033448285, -2.546088562373184150, 1.176098017510569305 ) ) ;
#7944 = DIRECTION ( 'NONE',  ( 0.000000000000000000, 0.000000000000000000, -1.000000000000000000 ) ) ;
#7945 = DIRECTION ( 'NONE',  ( -0.000000000000000000, -0.000000000000000000, 1.000000000000000000 ) ) ;
#7946 = CARTESIAN_POINT ( 'NONE',  ( -1.006616814747114486E-29, -2.568816543514388222E-44, -4.500000000000000888 ) ) ;
#7947 = CARTESIAN_POINT ( 'NONE',  ( -52.77438362643999881, 65.17411849586700612, -145.2984795835770058 ) ) ;
#7948 = LINE ( 'NONE', #11297, #12554 ) ;
#7949 = DIRECTION ( 'NONE',  ( -0.000000000000000000, -0.000000000000000000, 1.000000000000000000 ) ) ;
#7950 = AXIS2_PLACEMENT_3D ( 'NONE', #8716, #9799, #12298 ) ;
#7951 = VERTEX_POINT ( 'NONE', #3587 ) ;
#7952 = VECTOR ( 'NONE', #12695, 1000.000000000000000 ) ;
#7953 = SURFACE_SIDE_STYLE ('',( #14008 ) ) ;
#7954 = CARTESIAN_POINT ( 'NONE',  ( 3.639928100339127948, -0.5225000000000105116, 1.508827519571796394 ) ) ;
#7955 = ORIENTED_EDGE ( 'NONE', *, *, #11585, .T. ) ;
#7956 = CARTESIAN_POINT ( 'NONE',  ( -3.535952561574606801, -3.053750000000104770, -0.7042925846621640451 ) ) ;
#7957 = LINE ( 'NONE', #3305, #7952 ) ;
#7958 = AXIS2_PLACEMENT_3D ( 'NONE', #6258, #2437, #11902 ) ;
#7959 = LINE ( 'NONE', #6670, #4157 ) ;
#7960 = PLANE ( 'NONE',  #1837 ) ;
#7961 = CIRCLE ( 'NONE', #6015, 0.8000000000000176970 ) ;
#7962 = DIRECTION ( 'NONE',  ( 0.000000000000000000, -0.000000000000000000, 1.000000000000000000 ) ) ;
#7963 = CARTESIAN_POINT ( 'NONE',  ( 10.10406781373725771, -85.69524470659703752, 70.08979243323349806 ) ) ;
#7964 = EDGE_CURVE ( 'NONE', #12262, #13840, #1249, .T. ) ;
#7965 = DIRECTION ( 'NONE',  ( 0.000000000000000000, 0.000000000000000000, -1.000000000000000000 ) ) ;
#7966 = ORIENTED_EDGE ( 'NONE', *, *, #7343, .F. ) ;
#7967 = DIRECTION ( 'NONE',  ( -1.000000000000000000, 0.000000000000000000, 0.000000000000000000 ) ) ;
#7968 = EDGE_CURVE ( 'NONE', #5785, #9613, #7774, .T. ) ;
#7969 = ORIENTED_EDGE ( 'NONE', *, *, #7997, .T. ) ;
#7970 = AXIS2_PLACEMENT_3D ( 'NONE', #14057, #4442, #12661 ) ;
#7971 = ORIENTED_EDGE ( 'NONE', *, *, #9705, .T. ) ;
#7972 = CARTESIAN_POINT ( 'NONE',  ( -0.3378546177656731597, -4.319374999999974207, 3.421346328963576156 ) ) ;
#7973 = ORIENTED_EDGE ( 'NONE', *, *, #345, .F. ) ;
#7974 = EDGE_LOOP ( 'NONE', ( #12632, #4741 ) ) ;
#7975 = ORIENTED_EDGE ( 'NONE', *, *, #4313, .T. ) ;
#7976 = CARTESIAN_POINT ( 'NONE',  ( -3.504929897947095530, -5.452338562372976760, -1.061798670046178783 ) ) ;
#7977 = CONICAL_SURFACE ( 'NONE', #5024, 1732.050807568789651, 1.047197551196575871 ) ;
#7978 = CARTESIAN_POINT ( 'NONE',  ( 3.768993168962329054, -0.5381249999999744293, 1.141810966380977455 ) ) ;
#7979 = DIRECTION ( 'NONE',  ( 0.9961946980917452121, -3.779777825264101491E-17, 0.08715574274766160756 ) ) ;
#7980 = CARTESIAN_POINT ( 'NONE',  ( -0.7951559085591690668, -2.281249999999988010, -4.003048974988245412 ) ) ;
#7981 = DIRECTION ( 'NONE',  ( 0.000000000000000000, 1.000000000000000000, 0.000000000000000000 ) ) ;
#7982 = CARTESIAN_POINT ( 'NONE',  ( -86.77438362644100778, 99.17411849586700612, -182.2484795835770228 ) ) ;
#7983 = AXIS2_PLACEMENT_3D ( 'NONE', #7048, #1138, #8042 ) ;
#7984 = DIRECTION ( 'NONE',  ( 0.000000000000000000, 0.000000000000000000, -1.000000000000000000 ) ) ;
#7985 = CARTESIAN_POINT ( 'NONE',  ( -59.27438362644000591, 82.17411849586700612, -150.4984795835769944 ) ) ;
#7986 = EDGE_CURVE ( 'NONE', #8986, #8947, #13517, .T. ) ;
#7987 = CARTESIAN_POINT ( 'NONE',  ( -52.77438362643999881, 62.81621999649657084, -147.9984795835769944 ) ) ;
#7988 = LINE ( 'NONE', #553, #4794 ) ;
#7989 = VERTEX_POINT ( 'NONE', #9855 ) ;
#7990 = FACE_OUTER_BOUND ( 'NONE', #11115, .T. ) ;
#7991 = AXIS2_PLACEMENT_3D ( 'NONE', #5914, #8216, #4572 ) ;
#7992 = ORIENTED_EDGE ( 'NONE', *, *, #13299, .T. ) ;
#7993 = ORIENTED_EDGE ( 'NONE', *, *, #5058, .T. ) ;
#7994 = ORIENTED_EDGE ( 'NONE', *, *, #6526, .T. ) ;
#7995 = CARTESIAN_POINT ( 'NONE',  ( 57.41329019055577021, 5.000000000000001776, 125.5408111191910763 ) ) ;
#7996 = CARTESIAN_POINT ( 'NONE',  ( 1.614039610742502573, -4.413124999999970655, 3.021508266705727586 ) ) ;
#7997 = EDGE_CURVE ( 'NONE', #11281, #2023, #6406, .T. ) ;
#7998 = DIRECTION ( 'NONE',  ( 1.000000000000000000, 0.000000000000000000, 0.000000000000000000 ) ) ;
#7999 = DIRECTION ( 'NONE',  ( 0.000000000000000000, 0.000000000000000000, -1.000000000000000000 ) ) ;
#8000 = AXIS2_PLACEMENT_3D ( 'NONE', #10654, #4619, #9564 ) ;
#8001 = CARTESIAN_POINT ( 'NONE',  ( 33.35543536254877495, -19.31989681812820692, 0.000000000000000000 ) ) ;
#8002 = CARTESIAN_POINT ( 'NONE',  ( -69.77438362644001302, 82.17411849586700612, -85.04847958357700577 ) ) ;
#8003 = DIRECTION ( 'NONE',  ( 0.000000000000000000, 0.000000000000000000, -1.000000000000000000 ) ) ;
#8004 = CARTESIAN_POINT ( 'NONE',  ( -4.278680128878765032, -0.4995676945082698217, 0.4731733880612277177 ) ) ;
#8005 = CARTESIAN_POINT ( 'NONE',  ( -12.81835358098578403, 11.99999970914576330, -14.13358795631400611 ) ) ;
#8006 = EDGE_CURVE ( 'NONE', #13082, #3491, #9352, .T. ) ;
#8007 = AXIS2_PLACEMENT_3D ( 'NONE', #6843, #12885, #5922 ) ;
#8008 = VERTEX_POINT ( 'NONE', #5376 ) ;
#8009 = FACE_OUTER_BOUND ( 'NONE', #3443, .T. ) ;
#8010 = EDGE_CURVE ( 'NONE', #13047, #3975, #7632, .T. ) ;
#8011 = EDGE_LOOP ( 'NONE', ( #11528, #8703, #11409, #12078, #14645, #2894 ) ) ;
#8012 = EDGE_CURVE ( 'NONE', #11318, #11895, #5421, .T. ) ;
#8013 = ORIENTED_EDGE ( 'NONE', *, *, #11591, .F. ) ;
#8014 = LINE ( 'NONE', #4378, #15130 ) ;
#8015 = VECTOR ( 'NONE', #6241, 1000.000000000000114 ) ;
#8016 = VERTEX_POINT ( 'NONE', #12352 ) ;
#8017 = VECTOR ( 'NONE', #1928, 1000.000000000000000 ) ;
#8018 = CARTESIAN_POINT ( 'NONE',  ( 3.919974135967671636, -1.062500000000018652, -1.622483930095183213 ) ) ;
#8019 = ORIENTED_EDGE ( 'NONE', *, *, #7544, .F. ) ;
#8020 = CARTESIAN_POINT ( 'NONE',  ( -3.380984900159444528, -2.405463562373173936, -2.257326875190593274 ) ) ;
#8021 = EDGE_CURVE ( 'NONE', #11859, #134, #13661, .T. ) ;
#8022 = CARTESIAN_POINT ( 'NONE',  ( -15.50000000000000000, -0.4000000000005236034, -22.50000000000000000 ) ) ;
#8023 = DIRECTION ( 'NONE',  ( 0.000000000000000000, 0.000000000000000000, -1.000000000000000000 ) ) ;
#8024 = DIRECTION ( 'NONE',  ( 0.000000000000000000, 1.000000000000000000, 0.000000000000000000 ) ) ;
#8025 = VECTOR ( 'NONE', #3711, 1000.000000000000000 ) ;
#8026 = AXIS2_PLACEMENT_3D ( 'NONE', #15161, #1052, #10360 ) ;
#8027 = EDGE_CURVE ( 'NONE', #11570, #13566, #195, .T. ) ;
#8028 = CARTESIAN_POINT ( 'NONE',  ( 14.25000000000000000, -2.500000000000000000, -23.22168783648699986 ) ) ;
#8029 = DIRECTION ( 'NONE',  ( -2.551930889570659960E-15, 1.000000000000000000, 0.000000000000000000 ) ) ;
#8030 = DIRECTION ( 'NONE',  ( 0.000000000000000000, 0.000000000000000000, -1.000000000000000000 ) ) ;
#8031 =( LENGTH_UNIT ( ) NAMED_UNIT ( * ) SI_UNIT ( .MILLI., .METRE. ) );
#8032 = EDGE_LOOP ( 'NONE', ( #3171, #5616, #11078, #226 ) ) ;
#8033 = CARTESIAN_POINT ( 'NONE',  ( 0.3809421545653357000, -0.8193749999999933031, -3.882302026224181635 ) ) ;
#8034 = ORIENTED_EDGE ( 'NONE', *, *, #10095, .T. ) ;
#8035 = AXIS2_PLACEMENT_3D ( 'NONE', #13408, #11080, #11149 ) ;
#8036 = CIRCLE ( 'NONE', #6573, 4.000000000000000000 ) ;
#8037 = VECTOR ( 'NONE', #13139, 1000.000000000000000 ) ;
#8038 = CARTESIAN_POINT ( 'NONE',  ( 1.055499318045234114, -2.788125000000055476, -3.484140247641438926 ) ) ;
#8039 = LINE ( 'NONE', #743, #519 ) ;
#8040 = DIRECTION ( 'NONE',  ( -1.000000000000000000, -1.724434379501977811E-15, 0.000000000000000000 ) ) ;
#8041 = DIRECTION ( 'NONE',  ( -1.000000000000000000, 0.000000000000000000, 0.000000000000000000 ) ) ;
#8042 = DIRECTION ( 'NONE',  ( 0.000000000000000000, 0.000000000000000000, 1.000000000000000000 ) ) ;
#8043 = DIRECTION ( 'NONE',  ( 0.000000000000000000, -1.000000000000000000, -4.336808689942017736E-16 ) ) ;
#8044 = DIRECTION ( 'NONE',  ( -1.000000000000000000, 0.000000000000000000, 0.000000000000000000 ) ) ;
#8045 = TOROIDAL_SURFACE ( 'NONE', #2139, 11.50000000000000000, 1.000000000000000000 ) ;
#8046 = ORIENTED_EDGE ( 'NONE', *, *, #5346, .T. ) ;
#8047 = VECTOR ( 'NONE', #8926, 1000.000000000000114 ) ;
#8048 = CARTESIAN_POINT ( 'NONE',  ( 17.12895037488186389, 10.99999970914575620, 0.2687305842673423095 ) ) ;
#8049 = ORIENTED_EDGE ( 'NONE', *, *, #9332, .T. ) ;
#8050 = VERTEX_POINT ( 'NONE', #5295 ) ;
#8051 = CARTESIAN_POINT ( 'NONE',  ( 3.388605160257775584, -4.569374999999831211, 0.3324735777646721790 ) ) ;
#8052 = EDGE_LOOP ( 'NONE', ( #13483, #10154 ) ) ;
#8053 = ORIENTED_EDGE ( 'NONE', *, *, #2625, .F. ) ;
#8054 = EDGE_LOOP ( 'NONE', ( #4449, #14024, #4089, #10995 ) ) ;
#8055 = CARTESIAN_POINT ( 'NONE',  ( -3.506906588862749086, -6.499213562373093112, 0.000000000000000000 ) ) ;
#8056 = CARTESIAN_POINT ( 'NONE',  ( -2.210630411551929075, -0.2412499999998789502, 3.306558829207901340 ) ) ;
#8057 = CIRCLE ( 'NONE', #12525, 1.250000000000001110 ) ;
#8058 = DIRECTION ( 'NONE',  ( 0.000000000000000000, 0.000000000000000000, -1.000000000000000000 ) ) ;
#8059 = VECTOR ( 'NONE', #15247, 1000.000000000000000 ) ;
#8060 = CARTESIAN_POINT ( 'NONE',  ( 3.905735209131758534, -3.031249999999969802, -0.7758307200683374205 ) ) ;
#8061 = DIRECTION ( 'NONE',  ( 0.000000000000000000, 0.000000000000000000, -1.000000000000000000 ) ) ;
#8062 = EDGE_CURVE ( 'NONE', #502, #13047, #6611, .T. ) ;
#8063 = CARTESIAN_POINT ( 'NONE',  ( -4.785585838562203875, 2.054436331234722246, 0.7111221836281561570 ) ) ;
#8064 = DIRECTION ( 'NONE',  ( -1.000000000000000000, -1.541976423090494894E-16, 0.000000000000000000 ) ) ;
#8065 = CARTESIAN_POINT ( 'NONE',  ( 4.296275033669349597, -0.4995676945082477838, 5.261419468239855985E-16 ) ) ;
#8066 = FACE_BOUND ( 'NONE', #5707, .T. ) ;
#8067 = CARTESIAN_POINT ( 'NONE',  ( 16.33565937784172917, -0.3156604612126716614, -21.53909249377372959 ) ) ;
#8068 = CARTESIAN_POINT ( 'NONE',  ( -86.77438362644100778, 99.17411849586700612, -145.4984795835769944 ) ) ;
#8069 = ORIENTED_EDGE ( 'NONE', *, *, #14409, .F. ) ;
#8070 = LINE ( 'NONE', #5924, #11230 ) ;
#8071 = ORIENTED_EDGE ( 'NONE', *, *, #14086, .F. ) ;
#8072 = VERTEX_POINT ( 'NONE', #8851 ) ;
#8073 = VERTEX_POINT ( 'NONE', #13594 ) ;
#8074 = VECTOR ( 'NONE', #5732, 1000.000000000000000 ) ;
#8075 = DIRECTION ( 'NONE',  ( -0.08715574274766160756, 3.149814854386744309E-18, 0.9961946980917452121 ) ) ;
#8076 = PRODUCT_RELATED_PRODUCT_CATEGORY ( 'part', '', ( #1739 ) ) ;
#8077 = EDGE_CURVE ( 'NONE', #12917, #7621, #10601, .T. ) ;
#8078 = CARTESIAN_POINT ( 'NONE',  ( -2.669536895096369378, -4.194375000000057696, 2.192493760422927984 ) ) ;
#8079 = SURFACE_SIDE_STYLE ('',( #3346 ) ) ;
#8080 = CIRCLE ( 'NONE', #12059, 3.299999999999473577 ) ;
#8081 = LINE ( 'NONE', #12819, #5511 ) ;
#8082 = LINE ( 'NONE', #942, #6515 ) ;
#8083 = DIRECTION ( 'NONE',  ( 0.000000000000000000, 1.000000000000000000, 0.000000000000000000 ) ) ;
#8084 = AXIS2_PLACEMENT_3D ( 'NONE', #13756, #8939, #9239 ) ;
#8085 = CARTESIAN_POINT ( 'NONE',  ( -15.50000000000000000, 0.000000000000000000, 22.50000000000000000 ) ) ;
#8086 = DIRECTION ( 'NONE',  ( 0.000000000000000000, 1.000000000000000000, 0.000000000000000000 ) ) ;
#8087 = CIRCLE ( 'NONE', #5385, 3.000000000000002665 ) ;
#8088 = LINE ( 'NONE', #12824, #13751 ) ;
#8089 = CARTESIAN_POINT ( 'NONE',  ( -73.13733409597239188, 66.60412428008086749, -81.84847958357697451 ) ) ;
#8090 = ORIENTED_EDGE ( 'NONE', *, *, #14370, .T. ) ;
#8091 = LINE ( 'NONE', #2265, #10832 ) ;
#8092 = ORIENTED_EDGE ( 'NONE', *, *, #4793, .T. ) ;
#8093 = ORIENTED_EDGE ( 'NONE', *, *, #13202, .F. ) ;
#8094 = DIRECTION ( 'NONE',  ( 0.000000000000000000, 0.000000000000000000, -1.000000000000000000 ) ) ;
#8095 = AXIS2_PLACEMENT_3D ( 'NONE', #3916, #1510, #342 ) ;
#8096 = ORIENTED_EDGE ( 'NONE', *, *, #1755, .T. ) ;
#8097 = VECTOR ( 'NONE', #5828, 1000.000000000000000 ) ;
#8098 = CARTESIAN_POINT ( 'NONE',  ( 2.351042318464003689, -1.156249999999995559, -3.516557504029556913 ) ) ;
#8099 = ORIENTED_EDGE ( 'NONE', *, *, #6968, .T. ) ;
#8100 = EDGE_CURVE ( 'NONE', #1813, #2834, #3180, .T. ) ;
#8101 = CARTESIAN_POINT ( 'NONE',  ( 3.986784942675642540, -2.999213562373096220, 0.001049275647879016615 ) ) ;
#8102 = FACE_OUTER_BOUND ( 'NONE', #10707, .T. ) ;
#8103 = EDGE_CURVE ( 'NONE', #191, #389, #9361, .T. ) ;
#8104 = CARTESIAN_POINT ( 'NONE',  ( -69.77438362644001302, 82.17411849586700612, -152.4984795835769944 ) ) ;
#8105 = ADVANCED_FACE ( 'NONE', ( #5146 ), #4671, .T. ) ;
#8106 = CYLINDRICAL_SURFACE ( 'NONE', #8502, 4.499999999999997335 ) ;
#8107 = CIRCLE ( 'NONE', #5646, 2.400000000000001243 ) ;
#8108 = AXIS2_PLACEMENT_3D ( 'NONE', #10432, #5897, #14096 ) ;
#8109 = DIRECTION ( 'NONE',  ( 0.000000000000000000, 0.000000000000000000, 1.000000000000000000 ) ) ;
#8110 = VERTEX_POINT ( 'NONE', #13442 ) ;
#8111 = DIRECTION ( 'NONE',  ( 0.000000000000000000, 0.000000000000000000, -1.000000000000000000 ) ) ;
#8112 = CYLINDRICAL_SURFACE ( 'NONE', #4019, 1.500000000000001332 ) ;
#8113 = EDGE_CURVE ( 'NONE', #4822, #2764, #13837, .T. ) ;
#8114 = DIRECTION ( 'NONE',  ( -1.000000000000000222, -1.444447458290426890E-33, 1.110223024625156540E-16 ) ) ;
#8115 = ORIENTED_EDGE ( 'NONE', *, *, #13338, .T. ) ;
#8116 = CARTESIAN_POINT ( 'NONE',  ( -15.08565937784311473, -0.3156604612129270127, 21.29584399676446083 ) ) ;
#8117 = CARTESIAN_POINT ( 'NONE',  ( 1.493882881115754069, -0.7724999999999562217, -3.610279343491855641 ) ) ;
#8118 = ORIENTED_EDGE ( 'NONE', *, *, #9815, .T. ) ;
#8119 = EDGE_CURVE ( 'NONE', #14049, #1813, #12841, .T. ) ;
#8120 = AXIS2_PLACEMENT_3D ( 'NONE', #8464, #169, #11961 ) ;
#8121 = CARTESIAN_POINT ( 'NONE',  ( 1.740706783794652379, -2.413124999999917808, 3.253752085064650412 ) ) ;
#8122 = DIRECTION ( 'NONE',  ( 0.1802821511763431361, 0.1220014872200674283, -0.9760194583528146728 ) ) ;
#8123 = EDGE_CURVE ( 'NONE', #1795, #14279, #3675, .T. ) ;
#8124 = ADVANCED_FACE ( 'NONE', ( #2167 ), #11562, .F. ) ;
#8125 = DIRECTION ( 'NONE',  ( 1.000000000000000000, 0.000000000000000000, 0.000000000000000000 ) ) ;
#8126 = CARTESIAN_POINT ( 'NONE',  ( -48.27438362644000591, 99.17411849586700612, -86.49847958357699440 ) ) ;
#8127 = DIRECTION ( 'NONE',  ( 0.000000000000000000, -0.000000000000000000, 1.000000000000000000 ) ) ;
#8128 = DIRECTION ( 'NONE',  ( 0.000000000000000000, -4.336808689942017736E-16, 1.000000000000000000 ) ) ;
#8129 = FACE_OUTER_BOUND ( 'NONE', #12889, .T. ) ;
#8130 = CARTESIAN_POINT ( 'NONE',  ( 0.000000000000000000, -2.500000000000000000, 45.00000000000000000 ) ) ;
#8131 = AXIS2_PLACEMENT_3D ( 'NONE', #461, #599, #5126 ) ;
#8132 = VERTEX_POINT ( 'NONE', #3409 ) ;
#8133 = DIRECTION ( 'NONE',  ( -0.8660254037844485886, 0.000000000000000000, -0.4999999999999827360 ) ) ;
#8134 = VERTEX_POINT ( 'NONE', #14960 ) ;
#8135 = ORIENTED_EDGE ( 'NONE', *, *, #6475, .F. ) ;
#8136 = CARTESIAN_POINT ( 'NONE',  ( 2.991299100910195463, -4.663125000000096776, -1.600316903339956687 ) ) ;
#8137 = VERTEX_POINT ( 'NONE', #2239 ) ;
#8138 = EDGE_LOOP ( 'NONE', ( #3710, #7780, #12326, #9173, #5222 ) ) ;
#8139 = ORIENTED_EDGE ( 'NONE', *, *, #4658, .T. ) ;
#8140 = CARTESIAN_POINT ( 'NONE',  ( 0.7473096651600278362, -4.217963562373095776, -3.751860142188157887 ) ) ;
#8141 = CYLINDRICAL_SURFACE ( 'NONE', #9261, 10.49999999999999467 ) ;
#8142 = CONICAL_SURFACE ( 'NONE', #708, 4.500000000000000888, 1.396263401595466691 ) ;
#8143 = CARTESIAN_POINT ( 'NONE',  ( -69.77438362644001302, 82.17411849586700612, -79.49847958357700861 ) ) ;
#8144 = DIRECTION ( 'NONE',  ( -0.8660254037844482555, 0.000000000000000000, 0.4999999999999831801 ) ) ;
#8145 = CARTESIAN_POINT ( 'NONE',  ( -4.015299829665333498, 2.374507716408090996, 2.045296687396993107 ) ) ;
#8146 = CARTESIAN_POINT ( 'NONE',  ( -4.296391350416484123, -0.4995676945082700438, -1.627175273956673067E-05 ) ) ;
#8147 = DIRECTION ( 'NONE',  ( -1.000000000000000000, 0.000000000000000000, 0.000000000000000000 ) ) ;
#8148 = DIRECTION ( 'NONE',  ( 1.224646799147351975E-16, 1.000000000000000000, 0.000000000000000000 ) ) ;
#8149 = DIRECTION ( 'NONE',  ( -1.000000000000000000, 0.000000000000000000, 1.669238443041288662E-16 ) ) ;
#8150 = CARTESIAN_POINT ( 'NONE',  ( 3.341349309646173715, -4.553750000000432507, 0.6655201449779497569 ) ) ;
#8151 = CARTESIAN_POINT ( 'NONE',  ( -15.50000000000000000, -0.1999999999999999556, 22.50000000000000000 ) ) ;
#8152 = VERTEX_POINT ( 'NONE', #8996 ) ;
#8153 = DIRECTION ( 'NONE',  ( 0.000000000000000000, 0.000000000000000000, -1.000000000000000000 ) ) ;
#8154 = VERTEX_POINT ( 'NONE', #6840 ) ;
#8155 = AXIS2_PLACEMENT_3D ( 'NONE', #13850, #1825, #5568 ) ;
#8156 = ORIENTED_EDGE ( 'NONE', *, *, #5277, .F. ) ;
#8157 = ORIENTED_EDGE ( 'NONE', *, *, #673, .T. ) ;
#8158 = CARTESIAN_POINT ( 'NONE',  ( 3.341349309646173715, -4.553750000000432507, 0.6655201449779497569 ) ) ;
#8159 = CARTESIAN_POINT ( 'NONE',  ( -50.07438362644099783, 99.17411849586700612, -145.4984795835769944 ) ) ;
#8160 = CARTESIAN_POINT ( 'NONE',  ( -62.02799568714584666, 164.3482369917340122, -79.59847958357700293 ) ) ;
#8161 = CARTESIAN_POINT ( 'NONE',  ( -73.13733409597239188, 66.60412428008086749, -83.44847958357698303 ) ) ;
#8162 = DIRECTION ( 'NONE',  ( 0.000000000000000000, 0.000000000000000000, 1.000000000000000000 ) ) ;
#8163 = DIRECTION ( 'NONE',  ( 0.000000000000000000, 1.000000000000000000, 0.000000000000000000 ) ) ;
#8164 = CARTESIAN_POINT ( 'NONE',  ( -86.77438362644001302, 99.17411849586700612, -145.4984795835769660 ) ) ;
#8165 = DIRECTION ( 'NONE',  ( -1.000000000000000000, 0.000000000000000000, 0.000000000000000000 ) ) ;
#8166 = DIRECTION ( 'NONE',  ( 0.000000000000000000, 1.000000000000000000, 0.000000000000000000 ) ) ;
#8167 = EDGE_LOOP ( 'NONE', ( #3887, #10605 ) ) ;
#8168 = CYLINDRICAL_SURFACE ( 'NONE', #6876, 16.06499999999999773 ) ;
#8169 = EDGE_CURVE ( 'NONE', #6270, #8371, #114, .T. ) ;
#8170 = ORIENTED_EDGE ( 'NONE', *, *, #8404, .T. ) ;
#8171 = ORIENTED_EDGE ( 'NONE', *, *, #5650, .T. ) ;
#8172 = CARTESIAN_POINT ( 'NONE',  ( 0.000000000000000000, 0.000000000000000000, 0.000000000000000000 ) ) ;
#8173 = EDGE_LOOP ( 'NONE', ( #9365, #275, #9572, #15222 ) ) ;
#8174 = EDGE_CURVE ( 'NONE', #2678, #411, #927, .T. ) ;
#8175 = CARTESIAN_POINT ( 'NONE',  ( 0.8338062855310036658, -0.7812499999999443778, 4.197676506703500010 ) ) ;
#8176 = ORIENTED_EDGE ( 'NONE', *, *, #6869, .T. ) ;
#8177 = CARTESIAN_POINT ( 'NONE',  ( -1.147267920495149918, -3.296088562373144182, -3.777078554815655131 ) ) ;
#8178 = CARTESIAN_POINT ( 'NONE',  ( 22.58164641901421632, -2.121185358860712356, -11.99873403588350307 ) ) ;
#8179 = FACE_BOUND ( 'NONE', #8491, .T. ) ;
#8180 = CARTESIAN_POINT ( 'NONE',  ( 4.015299829665321063, 2.374507716408110536, -2.045296687396993107 ) ) ;
#8181 = CARTESIAN_POINT ( 'NONE',  ( -86.77438362643999881, 65.17411849586700612, -182.2484795835770228 ) ) ;
#8182 = VERTEX_POINT ( 'NONE', #5605 ) ;
#8183 = LINE ( 'NONE', #8260, #4887 ) ;
#8184 = EDGE_CURVE ( 'NONE', #15328, #3454, #7652, .T. ) ;
#8185 = FACE_OUTER_BOUND ( 'NONE', #10180, .T. ) ;
#8186 = VERTEX_POINT ( 'NONE', #4352 ) ;
#8187 = EDGE_CURVE ( 'NONE', #8759, #3945, #452, .T. ) ;
#8188 = CARTESIAN_POINT ( 'NONE',  ( 2.644209610478730266, -4.874999999999846345, 2.642267524923772370 ) ) ;
#8189 = EDGE_LOOP ( 'NONE', ( #13319, #986, #4359, #11639, #4765, #7704 ) ) ;
#8190 = CARTESIAN_POINT ( 'NONE',  ( -0.001340710925747373022, -2.834999999999994635, -3.634308738048381393 ) ) ;
#8191 = CARTESIAN_POINT ( 'NONE',  ( -69.77438362644001302, 79.67411849586700612, -51.99847958357699440 ) ) ;
#8192 = EDGE_CURVE ( 'NONE', #8567, #6471, #11392, .T. ) ;
#8193 = EDGE_CURVE ( 'NONE', #13653, #2626, #11851, .T. ) ;
#8194 = CARTESIAN_POINT ( 'NONE',  ( 16.75000000000000000, -0.2038245569916320166, -21.77831216351300014 ) ) ;
#8195 = DIRECTION ( 'NONE',  ( -2.065146995210485003E-17, -4.130293990420970006E-17, -1.000000000000000000 ) ) ;
#8196 = AXIS2_PLACEMENT_3D ( 'NONE', #6572, #2991, #7729 ) ;
#8197 = LINE ( 'NONE', #1214, #1951 ) ;
#8198 = DIRECTION ( 'NONE',  ( -0.9961946980917452121, 7.200509705930737227E-17, -0.08715574274766155205 ) ) ;
#8199 = EDGE_CURVE ( 'NONE', #7742, #5984, #1444, .T. ) ;
#8200 = DIRECTION ( 'NONE',  ( -1.000000000000000000, 0.000000000000000000, 0.000000000000000000 ) ) ;
#8201 = VECTOR ( 'NONE', #7376, 1000.000000000000114 ) ;
#8202 = EDGE_LOOP ( 'NONE', ( #15275, #5420 ) ) ;
#8203 = CARTESIAN_POINT ( 'NONE',  ( -69.77438362644001302, 82.17411849586700612, -152.4984795835769944 ) ) ;
#8204 = ORIENTED_EDGE ( 'NONE', *, *, #6232, .F. ) ;
#8205 = EDGE_CURVE ( 'NONE', #8552, #4318, #12601, .T. ) ;
#8206 = ORIENTED_EDGE ( 'NONE', *, *, #8298, .F. ) ;
#8207 = EDGE_CURVE ( 'NONE', #7422, #13506, #3251, .T. ) ;
#8208 = EDGE_LOOP ( 'NONE', ( #9083, #6367, #14087, #15312, #14197, #10776, #6880, #12339, #2543, #5927, #4718, #12785, #9919, #6327, #12282, #13448, #6744, #14724, #2813, #4990, #4188 ) ) ;
#8209 = ORIENTED_EDGE ( 'NONE', *, *, #6046, .F. ) ;
#8210 = VERTEX_POINT ( 'NONE', #13957 ) ;
#8211 = AXIS2_PLACEMENT_3D ( 'NONE', #11191, #6478, #6640 ) ;
#8212 = CARTESIAN_POINT ( 'NONE',  ( 3.390724153796742968, -4.077338562372932351, -1.811240771910064051 ) ) ;
#8213 = CARTESIAN_POINT ( 'NONE',  ( -52.77438362644000591, 65.17411849586700612, -79.59847958357700293 ) ) ;
#8214 = AXIS2_PLACEMENT_3D ( 'NONE', #11972, #3438, #7016 ) ;
#8215 = CARTESIAN_POINT ( 'NONE',  ( -3.452158817763116616, 2.307268873417411381, 3.020685531837380200 ) ) ;
#8216 = DIRECTION ( 'NONE',  ( -0.4999999999999832356, 0.000000000000000000, 0.8660254037844483666 ) ) ;
#8217 = LINE ( 'NONE', #1157, #11567 ) ;
#8218 = CARTESIAN_POINT ( 'NONE',  ( -62.02799568714584666, 60.67411849586701322, -152.4984795835769944 ) ) ;
#8219 = DIRECTION ( 'NONE',  ( -0.000000000000000000, 0.000000000000000000, 1.000000000000000000 ) ) ;
#8220 = CARTESIAN_POINT ( 'NONE',  ( 22.58164641901421632, -2.908542394189813650E-07, -0.3335879563140091153 ) ) ;
#8221 = DIRECTION ( 'NONE',  ( -1.000000000000000000, -2.548822376660340629E-15, 0.000000000000000000 ) ) ;
#8222 = EDGE_CURVE ( 'NONE', #13652, #9914, #2091, .T. ) ;
#8223 = CARTESIAN_POINT ( 'NONE',  ( -2.533829858540697977, -3.209999999999945786, 2.535703909530142575 ) ) ;
#8224 = CARTESIAN_POINT ( 'NONE',  ( -4.522482571421200248, -11.00000029085428110, 70.03692566716176771 ) ) ;
#8225 = CIRCLE ( 'NONE', #1286, 4.500000000000003553 ) ;
#8226 = ORIENTED_EDGE ( 'NONE', *, *, #6785, .T. ) ;
#8227 = DIRECTION ( 'NONE',  ( 1.000000000000000000, 0.000000000000000000, 0.000000000000000000 ) ) ;
#8228 = ORIENTED_EDGE ( 'NONE', *, *, #14693, .F. ) ;
#8229 =( GEOMETRIC_REPRESENTATION_CONTEXT ( 3 ) GLOBAL_UNCERTAINTY_ASSIGNED_CONTEXT ( ( #5307 ) ) GLOBAL_UNIT_ASSIGNED_CONTEXT ( ( #7134, #2457, #10604 ) ) REPRESENTATION_CONTEXT ( 'NONE', 'WORKASPACE' ) );
#8230 = ORIENTED_EDGE ( 'NONE', *, *, #7448, .F. ) ;
#8231 = ORIENTED_EDGE ( 'NONE', *, *, #8027, .F. ) ;
#8232 = DIRECTION ( 'NONE',  ( -0.003614861529253208996, 0.000000000000000000, 0.9999934663667179313 ) ) ;
#8233 = CARTESIAN_POINT ( 'NONE',  ( 1.394838545734166990, -2.772499999999996856, -3.364978284447634582 ) ) ;
#8234 = VECTOR ( 'NONE', #14638, 1000.000000000000000 ) ;
#8235 = CARTESIAN_POINT ( 'NONE',  ( 4.330127018922192761, 1.086454989718688594E-14, 1.499999999999999112 ) ) ;
#8236 = CARTESIAN_POINT ( 'NONE',  ( 3.654380903460823671, -4.968749999999916511, 0.7255053565382596492 ) ) ;
#8237 = DIRECTION ( 'NONE',  ( 0.000000000000000000, 0.000000000000000000, -1.000000000000000000 ) ) ;
#8238 = CARTESIAN_POINT ( 'NONE',  ( -84.07438362644101915, 99.17411849586700612, -145.2984795835770058 ) ) ;
#8239 = DIRECTION ( 'NONE',  ( 0.000000000000000000, 1.000000000000000000, 0.000000000000000000 ) ) ;
#8240 = CARTESIAN_POINT ( 'NONE',  ( -42.77438362644000591, 59.67411849586700612, -79.59847958357700293 ) ) ;
#8241 = DIRECTION ( 'NONE',  ( -1.000000000000000000, 0.000000000000000000, 0.000000000000000000 ) ) ;
#8242 = CIRCLE ( 'NONE', #555, 4.500000000000003553 ) ;
#8243 = DIRECTION ( 'NONE',  ( -0.000000000000000000, -0.000000000000000000, 1.000000000000000000 ) ) ;
#8244 = EDGE_LOOP ( 'NONE', ( #4547, #6420, #10089, #7577 ) ) ;
#8245 = PLANE ( 'NONE',  #672 ) ;
#8246 = ORIENTED_EDGE ( 'NONE', *, *, #14917, .F. ) ;
#8247 = ORIENTED_EDGE ( 'NONE', *, *, #6427, .F. ) ;
#8248 = CARTESIAN_POINT ( 'NONE',  ( -4.427870617159052280, 0.4999999999999987232, -3.710358631349437542E-13 ) ) ;
#8249 = ORIENTED_EDGE ( 'NONE', *, *, #3905, .T. ) ;
#8250 = VECTOR ( 'NONE', #15261, 1000.000000000000000 ) ;
#8251 = CARTESIAN_POINT ( 'NONE',  ( -3.470181165153897407, -1.592963562373082897, 2.317368808847834583 ) ) ;
#8252 = AXIS2_PLACEMENT_3D ( 'NONE', #6697, #11112, #14669 ) ;
#8253 = CARTESIAN_POINT ( 'NONE',  ( 10.10406781373725771, 10.99999970914572778, 69.08979243323354069 ) ) ;
#8254 = DIRECTION ( 'NONE',  ( 0.000000000000000000, 0.000000000000000000, 1.000000000000000000 ) ) ;
#8255 = VECTOR ( 'NONE', #8732, 1000.000000000000000 ) ;
#8256 = DIRECTION ( 'NONE',  ( 1.287488025362404182E-15, 1.000000000000000000, 0.000000000000000000 ) ) ;
#8257 = ADVANCED_FACE ( 'NONE', ( #6691 ), #12800, .T. ) ;
#8258 = CARTESIAN_POINT ( 'NONE',  ( 57.41329019055577021, 2.488961461112888074, 127.7236236191910734 ) ) ;
#8259 = ORIENTED_EDGE ( 'NONE', *, *, #3658, .T. ) ;
#8260 = CARTESIAN_POINT ( 'NONE',  ( -48.27438362644000591, 65.17411849586700612, -145.4984795835769660 ) ) ;
#8261 = CIRCLE ( 'NONE', #7537, 1.199999999999999734 ) ;
#8262 = AXIS2_PLACEMENT_3D ( 'NONE', #6603, #5436, #10134 ) ;
#8263 = FACE_OUTER_BOUND ( 'NONE', #4803, .T. ) ;
#8264 = ORIENTED_EDGE ( 'NONE', *, *, #6608, .T. ) ;
#8265 = CIRCLE ( 'NONE', #10994, 4.499999999999997335 ) ;
#8266 =( BOUNDED_CURVE ( )  B_SPLINE_CURVE ( 3, ( #11717, #4665, #1163, #8224 ),
 .UNSPECIFIED., .F., .T. ) 
 B_SPLINE_CURVE_WITH_KNOTS ( ( 4, 4 ),
 ( 1.570796326794897002, 3.141592653589793560 ),
 .UNSPECIFIED. ) 
 CURVE ( )  GEOMETRIC_REPRESENTATION_ITEM ( )  RATIONAL_B_SPLINE_CURVE ( ( 1.000000000000000000, 0.8047378541243649375, 0.8047378541243649375, 1.000000000000000000 ) ) 
 REPRESENTATION_ITEM ( '' )  );
#8267 = PRESENTATION_STYLE_ASSIGNMENT (( #3765 ) ) ;
#8268 = CARTESIAN_POINT ( 'NONE',  ( 2.968551569176787197, -4.109374999999867661, -2.434929705433495073 ) ) ;
#8269 = EDGE_LOOP ( 'NONE', ( #6382, #15007, #13465, #5206 ) ) ;
#8270 = PRODUCT_RELATED_PRODUCT_CATEGORY ( 'part', '', ( #5345 ) ) ;
#8271 = CARTESIAN_POINT ( 'NONE',  ( -3.335258087793214088, -3.022499999999893827, -1.380066378191329379 ) ) ;
#8272 = CIRCLE ( 'NONE', #1324, 3.499999999999999556 ) ;
#8273 = ADVANCED_FACE ( 'NONE', ( #4269 ), #11399, .F. ) ;
#8274 = AXIS2_PLACEMENT_3D ( 'NONE', #2535, #3780, #12942 ) ;
#8275 = CARTESIAN_POINT ( 'NONE',  ( 15.50000000000000000, -0.1999999999999999556, 22.50000000000000000 ) ) ;
#8276 = CARTESIAN_POINT ( 'NONE',  ( 6.573385150445030689, -3.618985300545107364, 6.000000000000000000 ) ) ;
#8277 = DIRECTION ( 'NONE',  ( 1.000000000000000000, 0.000000000000000000, 0.000000000000000000 ) ) ;
#8278 = DIRECTION ( 'NONE',  ( 1.000000000000000000, 0.000000000000000000, 0.000000000000000000 ) ) ;
#8279 = DIRECTION ( 'NONE',  ( -1.000000000000000000, -2.551930889570659565E-15, 0.000000000000000000 ) ) ;
#8280 = VERTEX_POINT ( 'NONE', #4964 ) ;
#8281 = CARTESIAN_POINT ( 'NONE',  ( -91.27438362643999881, 65.17411849586700612, -145.4984795835769660 ) ) ;
#8282 = VECTOR ( 'NONE', #12099, 1000.000000000000000 ) ;
#8283 = AXIS2_PLACEMENT_3D ( 'NONE', #976, #8195, #15087 ) ;
#8284 = ORIENTED_EDGE ( 'NONE', *, *, #3763, .F. ) ;
#8285 = EDGE_CURVE ( 'NONE', #7936, #9953, #1076, .T. ) ;
#8286 = CARTESIAN_POINT ( 'NONE',  ( -15.50000000000000000, -5.000000000000000000, 26.50000000000000000 ) ) ;
#8287 = ORIENTED_EDGE ( 'NONE', *, *, #673, .F. ) ;
#8288 = ORIENTED_EDGE ( 'NONE', *, *, #13857, .T. ) ;
#8289 = VERTEX_POINT ( 'NONE', #12027 ) ;
#8290 = CARTESIAN_POINT ( 'NONE',  ( 3.682145644596256151, -4.046088562373215680, -1.118437823483080296 ) ) ;
#8291 = DIRECTION ( 'NONE',  ( 0.000000000000000000, 0.000000000000000000, -1.000000000000000000 ) ) ;
#8292 = EDGE_CURVE ( 'NONE', #8472, #7286, #11868, .T. ) ;
#8293 = DIRECTION ( 'NONE',  ( -0.000000000000000000, 1.000000000000000000, -0.000000000000000000 ) ) ;
#8294 = AXIS2_PLACEMENT_3D ( 'NONE', #10053, #453, #6587 ) ;
#8295 = CARTESIAN_POINT ( 'NONE',  ( -3.250000000000014211, 7.362499999999993605, 3.980102097228917460E-16 ) ) ;
#8296 = CARTESIAN_POINT ( 'NONE',  ( -78.12438362644000733, 82.17411849586700612, -80.14847958357698587 ) ) ;
#8297 = EDGE_CURVE ( 'NONE', #1915, #4436, #4812, .T. ) ;
#8298 = EDGE_CURVE ( 'NONE', #6139, #3101, #14113, .T. ) ;
#8299 = CARTESIAN_POINT ( 'NONE',  ( -0.8655643756567900082, -2.325867345846483398E-15, 4.500000000000000000 ) ) ;
#8300 = CARTESIAN_POINT ( 'NONE',  ( -62.02799568714584666, 110.1741184958670061, -79.59847958357700293 ) ) ;
#8301 = CIRCLE ( 'NONE', #14248, 0.1999999999999987899 ) ;
#8302 = FACE_BOUND ( 'NONE', #7245, .T. ) ;
#8303 = CARTESIAN_POINT ( 'NONE',  ( 1.363531154075378282, -3.397500000000037712, 3.288412936073061399 ) ) ;
#8304 = CARTESIAN_POINT ( 'NONE',  ( -86.77438362644001302, 99.17411849586700612, -145.4984795835769660 ) ) ;
#8305 = ORIENTED_EDGE ( 'NONE', *, *, #13080, .T. ) ;
#8306 = LINE ( 'NONE', #153, #344 ) ;
#8307 = ORIENTED_EDGE ( 'NONE', *, *, #11227, .F. ) ;
#8308 = EDGE_CURVE ( 'NONE', #3516, #11145, #9116, .T. ) ;
#8309 = ORIENTED_EDGE ( 'NONE', *, *, #14835, .T. ) ;
#8310 = ORIENTED_EDGE ( 'NONE', *, *, #3377, .F. ) ;
#8311 = AXIS2_PLACEMENT_3D ( 'NONE', #6665, #13486, #2851 ) ;
#8312 = CIRCLE ( 'NONE', #12535, 2.000000000000001776 ) ;
#8313 = CARTESIAN_POINT ( 'NONE',  ( -83.02438362644100778, 99.17411849586700612, -150.4984795835770228 ) ) ;
#8314 = CIRCLE ( 'NONE', #1621, 3.750000000000003553 ) ;
#8315 = CARTESIAN_POINT ( 'NONE',  ( 2.950365215318619949, -3.491249999999835651, 1.969791294043586660 ) ) ;
#8316 = EDGE_CURVE ( 'NONE', #14071, #9085, #9601, .T. ) ;
#8317 = LINE ( 'NONE', #13062, #1407 ) ;
#8318 = CARTESIAN_POINT ( 'NONE',  ( 21.98164641901421135, -3.654316742536411589, 0.2664120436859909735 ) ) ;
#8319 = CARTESIAN_POINT ( 'NONE',  ( -101.2743836264399988, 60.67411849586700612, -15.85886927678779834 ) ) ;
#8320 = DIRECTION ( 'NONE',  ( 0.000000000000000000, 0.7071067811865441310, -0.7071067811865510144 ) ) ;
#8321 = DIRECTION ( 'NONE',  ( 0.000000000000000000, 0.000000000000000000, 1.000000000000000000 ) ) ;
#8322 = CARTESIAN_POINT ( 'NONE',  ( -69.77438362643999881, 89.17411849586052597, -43.99847958364157563 ) ) ;
#8323 = AXIS2_PLACEMENT_3D ( 'NONE', #10885, #6243, #7476 ) ;
#8324 = DIRECTION ( 'NONE',  ( -1.000000000000000000, 0.000000000000000000, 0.000000000000000000 ) ) ;
#8325 = CARTESIAN_POINT ( 'NONE',  ( -69.77438362644001302, 82.17411849586700612, -79.59847958357700293 ) ) ;
#8326 = DIRECTION ( 'NONE',  ( -0.000000000000000000, -0.000000000000000000, 1.000000000000000000 ) ) ;
#8327 = AXIS2_PLACEMENT_3D ( 'NONE', #14305, #7024, #11750 ) ;
#8328 = ORIENTED_EDGE ( 'NONE', *, *, #8297, .T. ) ;
#8329 = VECTOR ( 'NONE', #445, 1000.000000000000000 ) ;
#8330 = FACE_OUTER_BOUND ( 'NONE', #6885, .T. ) ;
#8331 = VERTEX_POINT ( 'NONE', #8218 ) ;
#8332 = APPLICATION_CONTEXT ( 'automotive_design' ) ;
#8333 = ORIENTED_EDGE ( 'NONE', *, *, #11101, .F. ) ;
#8334 = ORIENTED_EDGE ( 'NONE', *, *, #1335, .T. ) ;
#8335 = DIRECTION ( 'NONE',  ( 1.000000000000000000, -0.000000000000000000, -0.000000000000000000 ) ) ;
#8336 = CARTESIAN_POINT ( 'NONE',  ( -1.660422764420820929, -0.3125000000000191513, -4.011647887856864436 ) ) ;
#8337 = ORIENTED_EDGE ( 'NONE', *, *, #14754, .F. ) ;
#8338 = CIRCLE ( 'NONE', #14274, 2.577850803773722443 ) ;
#8339 = CARTESIAN_POINT ( 'NONE',  ( -0.001142616198797753811, -0.7492135623732086858, 4.284427141808827777 ) ) ;
#8340 = VECTOR ( 'NONE', #5700, 1000.000000000000000 ) ;
#8341 = CIRCLE ( 'NONE', #15002, 4.500000000000003553 ) ;
#8342 = CYLINDRICAL_SURFACE ( 'NONE', #8961, 4.250000000000003553 ) ;
#8343 = FACE_OUTER_BOUND ( 'NONE', #13600, .T. ) ;
#8344 = FACE_OUTER_BOUND ( 'NONE', #4704, .T. ) ;
#8345 = DIRECTION ( 'NONE',  ( 0.000000000000000000, 1.000000000000000000, 0.000000000000000000 ) ) ;
#8346 = ORIENTED_EDGE ( 'NONE', *, *, #8077, .F. ) ;
#8347 = VECTOR ( 'NONE', #1809, 1000.000000000000000 ) ;
#8348 = LINE ( 'NONE', #10657, #14041 ) ;
#8349 = CARTESIAN_POINT ( 'NONE',  ( 16.82707151287372227, 11.72089179802205727, 0.2761915063695380423 ) ) ;
#8350 = VECTOR ( 'NONE', #3480, 1000.000000000000000 ) ;
#8351 = APPLICATION_PROTOCOL_DEFINITION ( 'draft international standard', 'automotive_design', 1998, #2468 ) ;
#8352 = ORIENTED_EDGE ( 'NONE', *, *, #5065, .F. ) ;
#8353 = CARTESIAN_POINT ( 'NONE',  ( 2.130457310823663519, -4.156249999999911182, -3.186652721750134809 ) ) ;
#8354 = ORIENTED_EDGE ( 'NONE', *, *, #1996, .F. ) ;
#8355 = EDGE_CURVE ( 'NONE', #5961, #14071, #11102, .T. ) ;
#8356 = VECTOR ( 'NONE', #10033, 1000.000000000000000 ) ;
#8357 = CARTESIAN_POINT ( 'NONE',  ( -0.3768771888557862493, -1.319375000000004405, 3.816279424444235069 ) ) ;
#8358 = FACE_OUTER_BOUND ( 'NONE', #8533, .T. ) ;
#8359 = LINE ( 'NONE', #11847, #5942 ) ;
#8360 = DIRECTION ( 'NONE',  ( -2.551930889570659960E-15, 1.000000000000000000, 0.000000000000000000 ) ) ;
#8361 = CARTESIAN_POINT ( 'NONE',  ( -52.77438362644000591, 99.17411849586700612, -145.4984795835769660 ) ) ;
#8362 = ORIENTED_EDGE ( 'NONE', *, *, #10152, .T. ) ;
#8363 = LINE ( 'NONE', #15326, #12490 ) ;
#8364 = EDGE_CURVE ( 'NONE', #10174, #14946, #4924, .T. ) ;
#8365 = DIRECTION ( 'NONE',  ( 1.000000000000000000, 0.000000000000000000, 0.000000000000000000 ) ) ;
#8366 = ORIENTED_EDGE ( 'NONE', *, *, #14252, .F. ) ;
#8367 = VECTOR ( 'NONE', #15127, 1000.000000000000000 ) ;
#8368 = FACE_OUTER_BOUND ( 'NONE', #3212, .T. ) ;
#8369 = CARTESIAN_POINT ( 'NONE',  ( -1.990045403832507054, -3.241250000000046594, 2.976654046991287217 ) ) ;
#8370 = ORIENTED_EDGE ( 'NONE', *, *, #151, .T. ) ;
#8371 = VERTEX_POINT ( 'NONE', #3646 ) ;
#8372 = EDGE_CURVE ( 'NONE', #12263, #2643, #11411, .T. ) ;
#8373 = EDGE_LOOP ( 'NONE', ( #6182, #3403, #12888, #14106 ) ) ;
#8374 = PLANE ( 'NONE',  #7798 ) ;
#8375 = B_SPLINE_CURVE_WITH_KNOTS ( 'NONE', 3,
 ( #9925, #8849, #13659, #6688, #12505, #14737 ),
 .UNSPECIFIED., .F., .F.,
 ( 4, 2, 4 ),
 ( 1.820537833122031213, 2.555393473688635453, 3.290249114255239693 ),
 .UNSPECIFIED. ) ;
#8376 = CARTESIAN_POINT ( 'NONE',  ( -15.50000000000000000, -0.4000000000005236034, 22.50000000000000000 ) ) ;
#8377 = CARTESIAN_POINT ( 'NONE',  ( -90.85838362644101096, 99.17411849586700612, -147.9984795835769944 ) ) ;
#8378 = CONICAL_SURFACE ( 'NONE', #3422, 3.750000000000003553, 0.7853981633974476129 ) ;
#8379 = DIRECTION ( 'NONE',  ( 0.000000000000000000, 0.000000000000000000, -1.000000000000000000 ) ) ;
#8380 = CARTESIAN_POINT ( 'NONE',  ( 0.000000000000000000, 0.000000000000000000, -79.59847958357700293 ) ) ;
#8381 = DIRECTION ( 'NONE',  ( -1.000000000000000000, 0.000000000000000000, 0.000000000000000000 ) ) ;
#8382 = CARTESIAN_POINT ( 'NONE',  ( -3.313940955170693758, -4.131874999999921805, 1.004348227522835924 ) ) ;
#8383 = DIRECTION ( 'NONE',  ( 0.000000000000000000, 0.000000000000000000, -1.000000000000000000 ) ) ;
#8384 = ORIENTED_EDGE ( 'NONE', *, *, #3372, .F. ) ;
#8385 = CARTESIAN_POINT ( 'NONE',  ( -50.73238362643999722, 66.35306774555222376, -147.9984795835769944 ) ) ;
#8386 = ADVANCED_FACE ( 'NONE', ( #9448 ), #5669, .T. ) ;
#8387 = ORIENTED_EDGE ( 'NONE', *, *, #1449, .T. ) ;
#8388 = EDGE_LOOP ( 'NONE', ( #7955, #13355 ) ) ;
#8389 = ORIENTED_EDGE ( 'NONE', *, *, #10263, .F. ) ;
#8390 = ADVANCED_FACE ( 'NONE', ( #14338 ), #7380, .T. ) ;
#8391 = CARTESIAN_POINT ( 'NONE',  ( -15.50000000000000000, -0.2038245569916614930, -23.94337567297399971 ) ) ;
#8392 = CARTESIAN_POINT ( 'NONE',  ( 1.766265845880009788, -4.828125000000014211, 3.301533676270316686 ) ) ;
#8393 = DIRECTION ( 'NONE',  ( 1.000000000000000000, 0.000000000000000000, 0.000000000000000000 ) ) ;
#8394 = CARTESIAN_POINT ( 'NONE',  ( -0.8000000000000111466, 9.015594676761164550, 0.000000000000000000 ) ) ;
#8395 = ADVANCED_FACE ( 'NONE', ( #1232 ), #3714, .F. ) ;
#8396 = CARTESIAN_POINT ( 'NONE',  ( -69.77438362644001302, 82.17411849586700612, -112.9984795835769944 ) ) ;
#8397 = DIRECTION ( 'NONE',  ( 0.000000000000000000, -0.000000000000000000, 1.000000000000000000 ) ) ;
#8398 = DIRECTION ( 'NONE',  ( 0.8660254037844383745, -0.5000000000000003331, 0.000000000000000000 ) ) ;
#8399 = CARTESIAN_POINT ( 'NONE',  ( -15.50000000000000000, -5.000000000000000000, -22.50000000000000000 ) ) ;
#8400 = DIRECTION ( 'NONE',  ( 1.000000000000000000, 0.000000000000000000, 0.000000000000000000 ) ) ;
#8401 = VECTOR ( 'NONE', #7435, 1000.000000000000000 ) ;
#8402 = ORIENTED_EDGE ( 'NONE', *, *, #8838, .F. ) ;
#8403 = CARTESIAN_POINT ( 'NONE',  ( 17.04394838817069768, -11.40000029085424238, 0.2824263826447100945 ) ) ;
#8404 = EDGE_CURVE ( 'NONE', #11245, #8072, #5832, .T. ) ;
#8405 = ORIENTED_EDGE ( 'NONE', *, *, #8867, .F. ) ;
#8406 = VERTEX_POINT ( 'NONE', #145 ) ;
#8407 = CARTESIAN_POINT ( 'NONE',  ( -16.75000000000000000, -0.2038245569916330158, -21.77831216351300014 ) ) ;
#8408 = ADVANCED_FACE ( 'NONE', ( #8443 ), #5991, .F. ) ;
#8409 = EDGE_CURVE ( 'NONE', #4688, #6450, #7219, .T. ) ;
#8410 = ORIENTED_EDGE ( 'NONE', *, *, #8123, .F. ) ;
#8411 = CARTESIAN_POINT ( 'NONE',  ( -0.4082801294501576805, -1.733588562373098663, 4.134097036138766335 ) ) ;
#8412 = DIRECTION ( 'NONE',  ( -1.740799290094577062E-15, -1.000000000000000000, -6.292789498690070142E-18 ) ) ;
#8413 = LINE ( 'NONE', #4769, #15243 ) ;
#8414 = DIRECTION ( 'NONE',  ( -1.000000000000000000, 0.000000000000000000, 0.000000000000000000 ) ) ;
#8415 = CARTESIAN_POINT ( 'NONE',  ( 14.25000000000000000, -0.2038245569916330158, 21.77831216351300014 ) ) ;
#8416 = ORIENTED_EDGE ( 'NONE', *, *, #10875, .T. ) ;
#8417 = FACE_OUTER_BOUND ( 'NONE', #2082, .T. ) ;
#8418 = CARTESIAN_POINT ( 'NONE',  ( 17.04394838817069413, 11.39999970914576011, 0.2824263826447109826 ) ) ;
#8419 = APPLICATION_PROTOCOL_DEFINITION ( 'draft international standard', 'automotive_design', 1998, #12500 ) ;
#8420 = VERTEX_POINT ( 'NONE', #11942 ) ;
#8421 = CARTESIAN_POINT ( 'NONE',  ( -69.77438362644001302, 84.67411849586700612, -67.69567958357700377 ) ) ;
#8422 = CARTESIAN_POINT ( 'NONE',  ( -1.438726384651785040, -4.687499999999733546, 3.477001582427886817 ) ) ;
#8423 = ORIENTED_EDGE ( 'NONE', *, *, #5633, .T. ) ;
#8424 = CARTESIAN_POINT ( 'NONE',  ( -3.693744850241972077, -1.131875000000025722, 1.119430425315776523 ) ) ;
#8425 = DIRECTION ( 'NONE',  ( 0.000000000000000000, 0.000000000000000000, -1.000000000000000000 ) ) ;
#8426 = DIRECTION ( 'NONE',  ( 0.000000000000000000, 0.000000000000000000, -1.000000000000000000 ) ) ;
#8427 = LINE ( 'NONE', #6962, #13846 ) ;
#8428 = DIRECTION ( 'NONE',  ( -1.000000000000000000, 0.000000000000000000, 0.000000000000000000 ) ) ;
#8429 = FACE_OUTER_BOUND ( 'NONE', #7795, .T. ) ;
#8430 = ORIENTED_EDGE ( 'NONE', *, *, #10582, .F. ) ;
#8431 = CARTESIAN_POINT ( 'NONE',  ( 21.98164641901421135, 12.39999970914576188, -9.367156043074160721 ) ) ;
#8432 = EDGE_LOOP ( 'NONE', ( #7327, #2787, #2311, #11057 ) ) ;
#8433 = CARTESIAN_POINT ( 'NONE',  ( -64.53565528768383786, 67.29799558322736175, -83.44847958357698303 ) ) ;
#8434 = CARTESIAN_POINT ( 'NONE',  ( 3.389189273868537189, -3.538124999999807674, 1.026728768593258012 ) ) ;
#8435 = ORIENTED_EDGE ( 'NONE', *, *, #8440, .T. ) ;
#8436 = VERTEX_POINT ( 'NONE', #2634 ) ;
#8437 = EDGE_LOOP ( 'NONE', ( #9081, #3779, #1527, #5283 ) ) ;
#8438 = CARTESIAN_POINT ( 'NONE',  ( -15.50000000000000000, -1.037157890325000054, 22.50000000000000000 ) ) ;
#8439 = CARTESIAN_POINT ( 'NONE',  ( -73.64736697264332577, 89.17411849586700612, -58.99847958357700151 ) ) ;
#8440 = EDGE_CURVE ( 'NONE', #14968, #3175, #2549, .T. ) ;
#8441 = CARTESIAN_POINT ( 'NONE',  ( -84.73238362644100619, 100.3530677455522238, -147.9984795835769944 ) ) ;
#8442 = CIRCLE ( 'NONE', #2750, 8.000000000000007105 ) ;
#8443 = FACE_OUTER_BOUND ( 'NONE', #3157, .T. ) ;
#8444 = PRESENTATION_STYLE_ASSIGNMENT (( #4813 ) ) ;
#8445 = CARTESIAN_POINT ( 'NONE',  ( 1.403561989263864891E-14, -5.500000000000007994, 0.000000000000000000 ) ) ;
#8446 = ADVANCED_FACE ( 'NONE', ( #9837 ), #8378, .T. ) ;
#8447 = CARTESIAN_POINT ( 'NONE',  ( -0.9979582191391829227, -4.288125000000008846, 3.294238300096191452 ) ) ;
#8448 = LINE ( 'NONE', #6159, #1817 ) ;
#8449 = VERTEX_POINT ( 'NONE', #5198 ) ;
#8450 = CARTESIAN_POINT ( 'NONE',  ( -69.77438362644001302, 84.67411849586700612, -43.99847958357699440 ) ) ;
#8451 = ORIENTED_EDGE ( 'NONE', *, *, #9530, .F. ) ;
#8452 = CIRCLE ( 'NONE', #7723, 17.00000000000000000 ) ;
#8453 = VERTEX_POINT ( 'NONE', #1767 ) ;
#8454 = ORIENTED_EDGE ( 'NONE', *, *, #8600, .T. ) ;
#8455 = ORIENTED_EDGE ( 'NONE', *, *, #6623, .F. ) ;
#8456 = VECTOR ( 'NONE', #14675, 1000.000000000000000 ) ;
#8457 = FACE_OUTER_BOUND ( 'NONE', #6379, .T. ) ;
#8458 = FACE_OUTER_BOUND ( 'NONE', #2910, .T. ) ;
#8459 = ADVANCED_FACE ( 'NONE', ( #2778 ), #11008, .F. ) ;
#8460 = CARTESIAN_POINT ( 'NONE',  ( -69.77438362644001302, 82.17411849586700612, -138.4984795835769944 ) ) ;
#8461 = FACE_BOUND ( 'NONE', #8052, .T. ) ;
#8462 = ADVANCED_FACE ( 'NONE', ( #3013 ), #6517, .F. ) ;
#8463 = DIRECTION ( 'NONE',  ( -1.000000000000000000, -1.084202172485497334E-15, 0.000000000000000000 ) ) ;
#8464 = CARTESIAN_POINT ( 'NONE',  ( 21.98164641901421135, -12.40000029085423883, -9.367156043074160721 ) ) ;
#8465 = DIRECTION ( 'NONE',  ( 0.000000000000000000, 0.000000000000000000, -1.000000000000000000 ) ) ;
#8466 = CARTESIAN_POINT ( 'NONE',  ( -2.779367716467965987, 2.260916199238035267E-16, 50.11303170532691098 ) ) ;
#8467 = CARTESIAN_POINT ( 'NONE',  ( -65.90140028023257912, 89.17411849586700612, -29.37106258560738681 ) ) ;
#8468 = DIRECTION ( 'NONE',  ( 0.000000000000000000, 0.000000000000000000, -1.000000000000000000 ) ) ;
#8469 = EDGE_LOOP ( 'NONE', ( #14275, #15291, #14707, #14823, #6654 ) ) ;
#8470 = CARTESIAN_POINT ( 'NONE',  ( -69.77438362644001302, 82.17411849586700612, -67.69567958357700377 ) ) ;
#8471 = AXIS2_PLACEMENT_3D ( 'NONE', #8130, #908, #2072 ) ;
#8472 = VERTEX_POINT ( 'NONE', #5352 ) ;
#8473 = ORIENTED_EDGE ( 'NONE', *, *, #3562, .T. ) ;
#8474 = DIRECTION ( 'NONE',  ( -9.422394424380278809E-16, 1.000000000000000000, -0.000000000000000000 ) ) ;
#8475 = AXIS2_PLACEMENT_3D ( 'NONE', #6856, #2107, #2255 ) ;
#8476 = EDGE_CURVE ( 'NONE', #10367, #9170, #7415, .T. ) ;
#8477 = CARTESIAN_POINT ( 'NONE',  ( 4.200656737305518362, 0.04687500000002611800, 1.272606865360604189 ) ) ;
#8478 = EDGE_CURVE ( 'NONE', #4688, #1915, #1697, .T. ) ;
#8479 = CARTESIAN_POINT ( 'NONE',  ( -0.8351328658836442154, -0.7179635623729614391, 4.206420318747179365 ) ) ;
#8480 =( GEOMETRIC_REPRESENTATION_CONTEXT ( 3 ) GLOBAL_UNCERTAINTY_ASSIGNED_CONTEXT ( ( #13377 ) ) GLOBAL_UNIT_ASSIGNED_CONTEXT ( ( #11146, #1609, #4091 ) ) REPRESENTATION_CONTEXT ( 'NONE', 'WORKASPACE' ) );
#8481 = DIRECTION ( 'NONE',  ( 0.8660254037844383745, -0.5000000000000003331, 0.000000000000000000 ) ) ;
#8482 = DIRECTION ( 'NONE',  ( 0.000000000000000000, 0.000000000000000000, 1.000000000000000000 ) ) ;
#8483 = VECTOR ( 'NONE', #2256, 1000.000000000000000 ) ;
#8484 = ADVANCED_FACE ( 'NONE', ( #7531 ), #2940, .F. ) ;
#8485 = DIRECTION ( 'NONE',  ( 0.000000000000000000, 0.000000000000000000, -1.000000000000000000 ) ) ;
#8486 = FACE_OUTER_BOUND ( 'NONE', #4191, .T. ) ;
#8487 = EDGE_CURVE ( 'NONE', #9386, #7247, #1696, .T. ) ;
#8488 = STYLED_ITEM ( 'NONE', ( #13795 ), #10588 ) ;
#8489 = DIRECTION ( 'NONE',  ( -1.000000000000000000, 0.000000000000000000, 0.000000000000000000 ) ) ;
#8490 = EDGE_CURVE ( 'NONE', #8984, #3399, #7663, .T. ) ;
#8491 = EDGE_LOOP ( 'NONE', ( #9729, #4394, #8627, #3803, #12792, #5903 ) ) ;
#8492 = DIRECTION ( 'NONE',  ( 0.000000000000000000, 0.000000000000000000, 1.000000000000000000 ) ) ;
#8493 = CIRCLE ( 'NONE', #11964, 16.00000000000000000 ) ;
#8494 = ORIENTED_EDGE ( 'NONE', *, *, #689, .F. ) ;
#8495 = EDGE_CURVE ( 'NONE', #12591, #12773, #12361, .T. ) ;
#8496 = CARTESIAN_POINT ( 'NONE',  ( 1.826535687659961660, -3.828124999999970246, 3.419360526609917628 ) ) ;
#8497 = VERTEX_POINT ( 'NONE', #12405 ) ;
#8498 = VECTOR ( 'NONE', #5941, 1000.000000000000000 ) ;
#8499 = CARTESIAN_POINT ( 'NONE',  ( 3.931950937192209228, -0.5849999999998678479, -0.001434051515494208940 ) ) ;
#8500 = EDGE_CURVE ( 'NONE', #8132, #4034, #5874, .T. ) ;
#8501 = CARTESIAN_POINT ( 'NONE',  ( 21.98164641901421135, 11.99999970914576330, -11.73358795631400753 ) ) ;
#8502 = AXIS2_PLACEMENT_3D ( 'NONE', #12842, #10498, #2205 ) ;
#8503 = FACE_OUTER_BOUND ( 'NONE', #538, .T. ) ;
#8504 = AXIS2_PLACEMENT_3D ( 'NONE', #2810, #4135, #13601 ) ;
#8505 = DIRECTION ( 'NONE',  ( -1.000000000000000000, -2.551930889570659960E-15, 0.000000000000000000 ) ) ;
#8506 = DIRECTION ( 'NONE',  ( 0.5000000000000003331, 0.8660254037844384856, 0.000000000000000000 ) ) ;
#8507 = DIRECTION ( 'NONE',  ( 0.000000000000000000, 0.000000000000000000, -1.000000000000000000 ) ) ;
#8508 = CARTESIAN_POINT ( 'NONE',  ( -52.77438362644100067, 99.17411849586700612, -150.4984795835770228 ) ) ;
#8509 = ORIENTED_EDGE ( 'NONE', *, *, #12089, .T. ) ;
#8510 = CARTESIAN_POINT ( 'NONE',  ( -52.77438362644100067, 99.17411849586700612, -147.9984795835769944 ) ) ;
#8511 = DIRECTION ( 'NONE',  ( 0.000000000000000000, 0.000000000000000000, 1.000000000000000000 ) ) ;
#8512 = ORIENTED_EDGE ( 'NONE', *, *, #6202, .F. ) ;
#8513 = DIRECTION ( 'NONE',  ( 0.000000000000000000, 1.000000000000000000, 0.000000000000000000 ) ) ;
#8514 = CARTESIAN_POINT ( 'NONE',  ( 3.601230736643933117, -2.553749999999958220, 0.7149504581460883745 ) ) ;
#8515 = VERTEX_POINT ( 'NONE', #9194 ) ;
#8516 = ORIENTED_EDGE ( 'NONE', *, *, #8113, .T. ) ;
#8517 = CIRCLE ( 'NONE', #6062, 2.042000000000002036 ) ;
#8518 = CIRCLE ( 'NONE', #3554, 4.000000000000000000 ) ;
#8519 = ORIENTED_EDGE ( 'NONE', *, *, #2177, .T. ) ;
#8520 = DIRECTION ( 'NONE',  ( -0.000000000000000000, -0.000000000000000000, 1.000000000000000000 ) ) ;
#8521 = CARTESIAN_POINT ( 'NONE',  ( 26.62067127263865274, -1.924145975121151140E-15, 23.92684502045323924 ) ) ;
#8522 = LINE ( 'NONE', #144, #13491 ) ;
#8523 = CARTESIAN_POINT ( 'NONE',  ( -69.77438362644001302, 82.17411849586700612, -83.44847958357698303 ) ) ;
#8524 = FACE_OUTER_BOUND ( 'NONE', #5257, .T. ) ;
#8525 = AXIS2_PLACEMENT_3D ( 'NONE', #11250, #1634, #6385 ) ;
#8526 = CIRCLE ( 'NONE', #7055, 2.999999999999999112 ) ;
#8527 = CARTESIAN_POINT ( 'NONE',  ( 0.3508518002069317410, -3.350624999999907150, 3.548798009676430887 ) ) ;
#8528 = LINE ( 'NONE', #2637, #6084 ) ;
#8529 = ORIENTED_EDGE ( 'NONE', *, *, #7721, .T. ) ;
#8530 = LINE ( 'NONE', #8385, #7022 ) ;
#8531 = ORIENTED_EDGE ( 'NONE', *, *, #5246, .F. ) ;
#8532 = EDGE_LOOP ( 'NONE', ( #8860, #29 ) ) ;
#8533 = EDGE_LOOP ( 'NONE', ( #2142, #11098, #10979, #3690 ) ) ;
#8534 = ORIENTED_EDGE ( 'NONE', *, *, #14226, .T. ) ;
#8535 = LINE ( 'NONE', #9849, #2837 ) ;
#8536 = AXIS2_PLACEMENT_3D ( 'NONE', #14481, #2621, #11931 ) ;
#8537 = CARTESIAN_POINT ( 'NONE',  ( 0.6849063648203621568, -3.803749999999915143, -3.438650935610223947 ) ) ;
#8538 = EDGE_CURVE ( 'NONE', #12177, #3363, #11863, .T. ) ;
#8539 = VECTOR ( 'NONE', #3276, 1000.000000000000000 ) ;
#8540 = CARTESIAN_POINT ( 'NONE',  ( -104.2743836264399988, 0.000000000000000000, 0.000000000000000000 ) ) ;
#8541 = PLANE ( 'NONE',  #12687 ) ;
#8542 = CARTESIAN_POINT ( 'NONE',  ( 2.598076211353315124, 0.1227504548087477720, 4.500000000000000000 ) ) ;
#8543 = DIRECTION ( 'NONE',  ( -1.000000000000000000, -1.196012985618917554E-12, 0.000000000000000000 ) ) ;
#8544 = DIRECTION ( 'NONE',  ( 0.8660254037844383745, -0.5000000000000003331, 0.000000000000000000 ) ) ;
#8545 = DIRECTION ( 'NONE',  ( 0.000000000000000000, -0.1666666666666656582, -0.9860132971832695770 ) ) ;
#8546 = DIRECTION ( 'NONE',  ( 1.000000000000000000, 2.459952698498907718E-15, 0.000000000000000000 ) ) ;
#8547 = DIRECTION ( 'NONE',  ( 0.000000000000000000, 1.000000000000000000, 0.000000000000000000 ) ) ;
#8548 = ORIENTED_EDGE ( 'NONE', *, *, #4419, .F. ) ;
#8549 = CARTESIAN_POINT ( 'NONE',  ( 15.50000000000000000, 0.000000000000000000, 22.50000000000000000 ) ) ;
#8550 = ORIENTED_EDGE ( 'NONE', *, *, #5452, .F. ) ;
#8551 = VECTOR ( 'NONE', #13607, 1000.000000000000000 ) ;
#8552 = VERTEX_POINT ( 'NONE', #4474 ) ;
#8553 = VECTOR ( 'NONE', #5379, 1000.000000000000114 ) ;
#8554 = CARTESIAN_POINT ( 'NONE',  ( -3.189069343666966816, -6.084999999999998188, 0.000000000000000000 ) ) ;
#8555 = ADVANCED_FACE ( 'NONE', ( #5663, #827 ), #15015, .T. ) ;
#8556 = CARTESIAN_POINT ( 'NONE',  ( -3.599033699595752367, -0.4062500000000055511, -2.406188570379728553 ) ) ;
#8557 = CARTESIAN_POINT ( 'NONE',  ( 2.301140841363210399, -1.842963562373116204, 3.441202151216794292 ) ) ;
#8558 = EDGE_CURVE ( 'NONE', #10234, #11568, #6189, .T. ) ;
#8559 = DIRECTION ( 'NONE',  ( 0.000000000000000000, -1.000000000000000000, 0.000000000000000000 ) ) ;
#8560 = MECHANICAL_DESIGN_GEOMETRIC_PRESENTATION_REPRESENTATION (  '', ( #374 ), #9041 ) ;
#8561 = CARTESIAN_POINT ( 'NONE',  ( -16.54633693294650953, -0.2717122460102549542, 21.66072723692568402 ) ) ;
#8562 = CARTESIAN_POINT ( 'NONE',  ( 14.45366306705349402, -0.2717122460102546766, -23.33927276307431598 ) ) ;
#8563 = AXIS2_PLACEMENT_3D ( 'NONE', #9579, #4492, #10908 ) ;
#8564 = DIRECTION ( 'NONE',  ( -9.422394424380278809E-16, 1.000000000000000000, -0.000000000000000000 ) ) ;
#8565 = CIRCLE ( 'NONE', #1879, 2.042000000000002036 ) ;
#8566 = CARTESIAN_POINT ( 'NONE',  ( 23.25000000000000000, 0.000000000000000000, -27.00000000000000000 ) ) ;
#8567 = VERTEX_POINT ( 'NONE', #3087 ) ;
#8568 = CARTESIAN_POINT ( 'NONE',  ( 0.000000000000000000, 0.000000000000000000, 0.000000000000000000 ) ) ;
#8569 = VECTOR ( 'NONE', #13213, 1000.000000000000000 ) ;
#8570 = ADVANCED_FACE ( 'NONE', ( #10287 ), #4421, .F. ) ;
#8571 = ORIENTED_EDGE ( 'NONE', *, *, #9332, .F. ) ;
#8572 = VECTOR ( 'NONE', #7572, 1000.000000000000000 ) ;
#8573 = SURFACE_SIDE_STYLE ('',( #11759 ) ) ;
#8574 = CARTESIAN_POINT ( 'NONE',  ( -3.630950894689927821, -4.453124999999883649, -1.099983568547476143 ) ) ;
#8575 = EDGE_LOOP ( 'NONE', ( #10923, #10571, #9661, #10815 ) ) ;
#8576 = CARTESIAN_POINT ( 'NONE',  ( 3.193773564512591090, -4.092963562373205022, -2.135702085600666322 ) ) ;
#8577 = EDGE_CURVE ( 'NONE', #8597, #11302, #2445, .T. ) ;
#8578 = ADVANCED_FACE ( 'NONE', ( #1923 ), #5430, .T. ) ;
#8579 = CARTESIAN_POINT ( 'NONE',  ( -86.77438362643999881, 62.81621999649657084, -147.9984795835769944 ) ) ;
#8580 = CARTESIAN_POINT ( 'NONE',  ( -35.58670980944424400, 5.000000000000001776, 93.54081111919107627 ) ) ;
#8581 = LINE ( 'NONE', #12389, #4035 ) ;
#8582 = B_SPLINE_CURVE_WITH_KNOTS ( 'NONE', 3,
 ( #4273, #6767, #14883, #703, #13822, #627 ),
 .UNSPECIFIED., .F., .F.,
 ( 4, 2, 4 ),
 ( 0.0002380763768131538560, 0.7291065797294589146, 1.457975083082104550 ),
 .UNSPECIFIED. ) ;
#8583 = CIRCLE ( 'NONE', #5622, 6.999999999974082954 ) ;
#8584 = CARTESIAN_POINT ( 'NONE',  ( -52.77438362644100067, 99.17411849586700612, -150.4984795835770228 ) ) ;
#8585 = AXIS2_PLACEMENT_3D ( 'NONE', #3350, #8083, #5853 ) ;
#8586 = ADVANCED_FACE ( 'NONE', ( #10129 ), #8142, .T. ) ;
#8587 = CARTESIAN_POINT ( 'NONE',  ( 22.58164641901421632, -12.00000029085423314, -14.73358795631400575 ) ) ;
#8588 = DIRECTION ( 'NONE',  ( 1.000000000000000000, 0.000000000000000000, 0.000000000000000000 ) ) ;
#8589 = LINE ( 'NONE', #8656, #1392 ) ;
#8590 = FACE_OUTER_BOUND ( 'NONE', #91, .T. ) ;
#8591 = ORIENTED_EDGE ( 'NONE', *, *, #4774, .T. ) ;
#8592 = VERTEX_POINT ( 'NONE', #14860 ) ;
#8593 = EDGE_CURVE ( 'NONE', #7307, #9134, #11365, .T. ) ;
#8594 = ORIENTED_EDGE ( 'NONE', *, *, #14629, .F. ) ;
#8595 = ORIENTED_EDGE ( 'NONE', *, *, #4620, .F. ) ;
#8596 = CARTESIAN_POINT ( 'NONE',  ( 1.055499318045256540, -2.788125000000055476, -3.484140247641439370 ) ) ;
#8597 = VERTEX_POINT ( 'NONE', #4330 ) ;
#8598 = AXIS2_PLACEMENT_3D ( 'NONE', #12617, #1979, #9038 ) ;
#8599 = ORIENTED_EDGE ( 'NONE', *, *, #3448, .F. ) ;
#8600 = EDGE_CURVE ( 'NONE', #3986, #1856, #11540, .T. ) ;
#8601 = CIRCLE ( 'NONE', #4890, 4.499999999999997335 ) ;
#8602 = EDGE_CURVE ( 'NONE', #2078, #1481, #13361, .T. ) ;
#8603 = CARTESIAN_POINT ( 'NONE',  ( -2.729504910555624608, -5.227506838825849655, -2.243639822945930007 ) ) ;
#8604 = CARTESIAN_POINT ( 'NONE',  ( -69.77438362644001302, 82.17411849586700612, -138.4984795835769944 ) ) ;
#8605 = CARTESIAN_POINT ( 'NONE',  ( -2.123244931150037651, -0.4995676945082646037, -3.627165614345276179 ) ) ;
#8606 = VECTOR ( 'NONE', #9326, 1000.000000000000114 ) ;
#8607 = CARTESIAN_POINT ( 'NONE',  ( -54.81638362644100226, 97.99516924618178848, -147.9984795835769944 ) ) ;
#8608 = DIRECTION ( 'NONE',  ( 1.000000000000000000, 0.000000000000000000, 0.000000000000000000 ) ) ;
#8609 = CIRCLE ( 'NONE', #429, 1.449999999999996403 ) ;
#8610 = EDGE_LOOP ( 'NONE', ( #5005, #14441, #7019, #9096, #13335 ) ) ;
#8611 = DIRECTION ( 'NONE',  ( -1.000000000000000000, 0.000000000000000000, 0.000000000000000000 ) ) ;
#8612 = ORIENTED_EDGE ( 'NONE', *, *, #416, .T. ) ;
#8613 = ORIENTED_EDGE ( 'NONE', *, *, #11226, .F. ) ;
#8614 = ORIENTED_EDGE ( 'NONE', *, *, #10146, .F. ) ;
#8615 = ORIENTED_EDGE ( 'NONE', *, *, #620, .F. ) ;
#8616 =( NAMED_UNIT ( * ) PLANE_ANGLE_UNIT ( ) SI_UNIT ( $, .RADIAN. ) );
#8617 = CARTESIAN_POINT ( 'NONE',  ( -0.3862366009529625832, -3.265625000000082601, -3.932116680993492874 ) ) ;
#8618 = LINE ( 'NONE', #9691, #11703 ) ;
#8619 = DIRECTION ( 'NONE',  ( 1.000000000000000000, 0.000000000000000000, 0.000000000000000000 ) ) ;
#8620 = DIRECTION ( 'NONE',  ( 1.000000000000000000, 0.000000000000000000, 0.000000000000000000 ) ) ;
#8621 = DIRECTION ( 'NONE',  ( -1.000000000000000000, 0.000000000000000000, 0.000000000000000000 ) ) ;
#8622 = DIRECTION ( 'NONE',  ( 2.551930889570659960E-15, -1.000000000000000000, -0.000000000000000000 ) ) ;
#8623 = CARTESIAN_POINT ( 'NONE',  ( -15.50000000000000000, -2.500000000000000000, 23.94337567297399971 ) ) ;
#8624 = FACE_OUTER_BOUND ( 'NONE', #1443, .T. ) ;
#8625 = ORIENTED_EDGE ( 'NONE', *, *, #11200, .T. ) ;
#8626 = CARTESIAN_POINT ( 'NONE',  ( -15.50000000000000000, -0.1999999999999999556, -23.94999999999999929 ) ) ;
#8627 = ORIENTED_EDGE ( 'NONE', *, *, #5370, .T. ) ;
#8628 = AXIS2_PLACEMENT_3D ( 'NONE', #766, #5917, #1158 ) ;
#8629 = ORIENTED_EDGE ( 'NONE', *, *, #11135, .T. ) ;
#8630 = CARTESIAN_POINT ( 'NONE',  ( 3.252598188045254801, -5.600624999999989306, -0.3215848719029840153 ) ) ;
#8631 = CARTESIAN_POINT ( 'NONE',  ( -72.45546847960517312, 89.83357606928413475, -58.65793715699411592 ) ) ;
#8632 = CARTESIAN_POINT ( 'NONE',  ( 3.013463120154616703, -5.647500000000105658, -1.249542180252701584 ) ) ;
#8633 = DIRECTION ( 'NONE',  ( 0.000000000000000000, 0.000000000000000000, -1.000000000000000000 ) ) ;
#8634 = FACE_OUTER_BOUND ( 'NONE', #1130, .T. ) ;
#8635 = AXIS2_PLACEMENT_3D ( 'NONE', #6673, #11380, #746 ) ;
#8636 = CARTESIAN_POINT ( 'NONE',  ( -15.50000000000000000, -5.000000000000000000, 22.50000000000000000 ) ) ;
#8637 = ADVANCED_FACE ( 'NONE', ( #3310 ), #12561, .F. ) ;
#8638 = CARTESIAN_POINT ( 'NONE',  ( 22.58164641901421632, -12.00000029085424202, -0.3335879563140091153 ) ) ;
#8639 = EDGE_LOOP ( 'NONE', ( #13842, #15003, #753, #3824 ) ) ;
#8640 = DIRECTION ( 'NONE',  ( -0.000000000000000000, 1.000000000000000000, -0.000000000000000000 ) ) ;
#8641 = EDGE_CURVE ( 'NONE', #6629, #15063, #5503, .T. ) ;
#8642 = CONTEXT_DEPENDENT_SHAPE_REPRESENTATION ( #10695, #13642 ) ;
#8643 = ORIENTED_EDGE ( 'NONE', *, *, #10286, .T. ) ;
#8644 = VECTOR ( 'NONE', #2924, 1000.000000000000000 ) ;
#8645 =( NAMED_UNIT ( * ) SI_UNIT ( $, .STERADIAN. ) SOLID_ANGLE_UNIT ( ) );
#8646 = CARTESIAN_POINT ( 'NONE',  ( 3.303237764219515427, -3.093750000000110578, -2.208893390251179589 ) ) ;
#8647 = VERTEX_POINT ( 'NONE', #12626 ) ;
#8648 = CARTESIAN_POINT ( 'NONE',  ( -3.788356809919846580, -4.499213562373157060, -0.0009870486262349110682 ) ) ;
#8649 = CARTESIAN_POINT ( 'NONE',  ( -1.470831194960214861, -1.272500000000085230, 3.548278161707651090 ) ) ;
#8650 = DIRECTION ( 'NONE',  ( 3.996802888650560011E-13, -1.000000000000000000, 0.000000000000000000 ) ) ;
#8651 = LINE ( 'NONE', #8810, #4776 ) ;
#8652 = EDGE_CURVE ( 'NONE', #6998, #13840, #1455, .T. ) ;
#8653 = DIRECTION ( 'NONE',  ( 0.000000000000000000, -0.1240337885538713436, 0.9922779949676268085 ) ) ;
#8654 = CARTESIAN_POINT ( 'NONE',  ( -12.81835358098578759, -11.40000029085423883, -8.183940086454239093 ) ) ;
#8655 = DIRECTION ( 'NONE',  ( 0.000000000000000000, 0.000000000000000000, -1.000000000000000000 ) ) ;
#8656 = CARTESIAN_POINT ( 'NONE',  ( -15.50000000000000000, -2.500000000000000000, -23.94337567297399971 ) ) ;
#8657 = CARTESIAN_POINT ( 'NONE',  ( -90.85838362644000199, 65.17411849586700612, -147.9984795835769944 ) ) ;
#8658 = EDGE_CURVE ( 'NONE', #10868, #2784, #8359, .T. ) ;
#8659 = DIRECTION ( 'NONE',  ( -1.000000000000000000, 0.000000000000000000, -0.000000000000000000 ) ) ;
#8660 = VERTEX_POINT ( 'NONE', #7128 ) ;
#8661 = ORIENTED_EDGE ( 'NONE', *, *, #7820, .F. ) ;
#8662 = ORIENTED_EDGE ( 'NONE', *, *, #12434, .F. ) ;
#8663 = DIRECTION ( 'NONE',  ( -1.000000000000000000, 0.000000000000000000, 0.000000000000000000 ) ) ;
#8664 = CARTESIAN_POINT ( 'NONE',  ( 1.033118776976111652, -3.381875000000070131, 3.408891928937247240 ) ) ;
#8665 = ORIENTED_EDGE ( 'NONE', *, *, #3849, .T. ) ;
#8666 = ORIENTED_EDGE ( 'NONE', *, *, #4326, .F. ) ;
#8667 = CARTESIAN_POINT ( 'NONE',  ( -1.336190917661197242, -3.897499999999990195, -3.228188129988408317 ) ) ;
#8668 = EDGE_CURVE ( 'NONE', #13430, #8289, #8427, .T. ) ;
#8669 = ADVANCED_FACE ( 'NONE', ( #11768 ), #14098, .F. ) ;
#8670 = CARTESIAN_POINT ( 'NONE',  ( 21.98164641901421135, -11.40000029085424238, -0.3335879563140091153 ) ) ;
#8671 = FACE_OUTER_BOUND ( 'NONE', #2788, .T. ) ;
#8672 = ADVANCED_FACE ( 'NONE', ( #4875 ), #7172, .T. ) ;
#8673 = PLANE ( 'NONE',  #9262 ) ;
#8674 = DIRECTION ( 'NONE',  ( -1.000000000000000000, -2.551930889570659960E-15, 0.000000000000000000 ) ) ;
#8675 = CARTESIAN_POINT ( 'NONE',  ( 14.25000000000000000, -0.2038245569916330158, -21.77831216351300014 ) ) ;
#8676 = CARTESIAN_POINT ( 'NONE',  ( -87.79538362643998539, 66.94254237039483257, -147.9984795835769944 ) ) ;
#8677 = EDGE_CURVE ( 'NONE', #7517, #1574, #1369, .T. ) ;
#8678 = FACE_OUTER_BOUND ( 'NONE', #14767, .T. ) ;
#8679 = ADVANCED_FACE ( 'NONE', ( #14164 ), #2297, .T. ) ;
#8680 = ORIENTED_EDGE ( 'NONE', *, *, #4976, .T. ) ;
#8681 = DIRECTION ( 'NONE',  ( 0.000000000000000000, 0.000000000000000000, 1.000000000000000000 ) ) ;
#8682 = VERTEX_POINT ( 'NONE', #2529 ) ;
#8683 = EDGE_LOOP ( 'NONE', ( #11827, #5674 ) ) ;
#8684 = ORIENTED_EDGE ( 'NONE', *, *, #1189, .T. ) ;
#8685 = EDGE_LOOP ( 'NONE', ( #7831, #3956, #3078 ) ) ;
#8686 = ORIENTED_EDGE ( 'NONE', *, *, #15198, .T. ) ;
#8687 = CARTESIAN_POINT ( 'NONE',  ( 37.35543536254874653, -19.31989681812820692, 6.000000000000001776 ) ) ;
#8688 = CARTESIAN_POINT ( 'NONE',  ( 2.337649614532405717, -2.444375000000051479, 2.849939602875970035 ) ) ;
#8689 = CARTESIAN_POINT ( 'NONE',  ( -50.73238362644099197, 100.3530677455522238, -147.9984795835769944 ) ) ;
#8690 = CARTESIAN_POINT ( 'NONE',  ( -2.667345689317278890, -4.625000000000156319, 2.665957393838279010 ) ) ;
#8691 = CARTESIAN_POINT ( 'NONE',  ( 0.000000000000000000, 0.000000000000000000, 0.000000000000000000 ) ) ;
#8692 = EDGE_CURVE ( 'NONE', #15148, #10983, #8197, .T. ) ;
#8693 = CYLINDRICAL_SURFACE ( 'NONE', #11061, 0.8000000000000113687 ) ;
#8694 = DIRECTION ( 'NONE',  ( 1.000000000000000000, 1.067522139062645347E-15, 0.000000000000000000 ) ) ;
#8695 = CARTESIAN_POINT ( 'NONE',  ( 17.18164641901421419, 11.39999970914575833, 0.2664120436859911956 ) ) ;
#8696 = DIRECTION ( 'NONE',  ( 0.000000000000000000, 0.000000000000000000, -1.000000000000000000 ) ) ;
#8697 = CARTESIAN_POINT ( 'NONE',  ( -50.07438362644099783, 99.17411849586700612, -145.2984795835770058 ) ) ;
#8698 = CARTESIAN_POINT ( 'NONE',  ( -69.77438362644001302, 82.17411849586700612, -80.14847958357698587 ) ) ;
#8699 = AXIS2_PLACEMENT_3D ( 'NONE', #12213, #14376, #5233 ) ;
#8700 = VERTEX_POINT ( 'NONE', #12935 ) ;
#8701 = DIRECTION ( 'NONE',  ( 1.000000000000000000, -0.000000000000000000, -0.000000000000000000 ) ) ;
#8702 = VERTEX_POINT ( 'NONE', #4945 ) ;
#8703 = ORIENTED_EDGE ( 'NONE', *, *, #12740, .T. ) ;
#8704 = EDGE_LOOP ( 'NONE', ( #8531, #10593, #10487 ) ) ;
#8705 = CARTESIAN_POINT ( 'NONE',  ( -2.276987973263314480, -5.960000000000099440, -2.278132229539954867 ) ) ;
#8706 = DIRECTION ( 'NONE',  ( 0.000000000000000000, 0.000000000000000000, 1.000000000000000000 ) ) ;
#8707 = CARTESIAN_POINT ( 'NONE',  ( 1.804507757947478197, -5.741250000000162501, -2.702832914148806331 ) ) ;
#8708 = CIRCLE ( 'NONE', #12921, 4.000000000000000000 ) ;
#8709 = CARTESIAN_POINT ( 'NONE',  ( -38.27438362644000591, 57.67411849586700612, -67.49847958357700861 ) ) ;
#8710 = CARTESIAN_POINT ( 'NONE',  ( 15.08757311576526128, -0.3152598339554911200, -23.70526090034004341 ) ) ;
#8711 = B_SPLINE_CURVE_WITH_KNOTS ( 'NONE', 3,
 ( #8982, #8756, #14722, #3955, #13423, #12337 ),
 .UNSPECIFIED., .F., .F.,
 ( 4, 2, 4 ),
 ( 0.0002380763768114607659, 0.7291065797294573603, 1.457975083082103218 ),
 .UNSPECIFIED. ) ;
#8712 = VECTOR ( 'NONE', #13379, 1000.000000000000000 ) ;
#8713 = CYLINDRICAL_SURFACE ( 'NONE', #10324, 2.000000000000001776 ) ;
#8714 = DIRECTION ( 'NONE',  ( 1.000000000000000000, 0.000000000000000000, 0.000000000000000000 ) ) ;
#8715 = AXIS2_PLACEMENT_3D ( 'NONE', #4316, #6729, #5492 ) ;
#8716 = CARTESIAN_POINT ( 'NONE',  ( 21.98164641901421135, 12.59999970914575940, -8.183940086454237317 ) ) ;
#8717 = VERTEX_POINT ( 'NONE', #6131 ) ;
#8718 = DIRECTION ( 'NONE',  ( 9.422394424380278809E-16, -1.000000000000000000, 0.000000000000000000 ) ) ;
#8719 = VECTOR ( 'NONE', #4965, 1000.000000000000000 ) ;
#8720 = ORIENTED_EDGE ( 'NONE', *, *, #4490, .F. ) ;
#8721 = CARTESIAN_POINT ( 'NONE',  ( -1.629699455448989389E-14, 8.699999999999999289, 5.655858585055787181E-29 ) ) ;
#8722 = CARTESIAN_POINT ( 'NONE',  ( -4.034970194612536254, -2.484375000000152767, -0.3959303163385184399 ) ) ;
#8723 = ORIENTED_EDGE ( 'NONE', *, *, #4502, .T. ) ;
#8724 = CARTESIAN_POINT ( 'NONE',  ( -3.020162574906126274, -3.608588562373100661, 2.477258684347839246 ) ) ;
#8725 = CARTESIAN_POINT ( 'NONE',  ( 22.58164641901421632, -11.40000029085424238, -0.3335879563140091153 ) ) ;
#8726 = EDGE_CURVE ( 'NONE', #13967, #160, #12115, .T. ) ;
#8727 = DIRECTION ( 'NONE',  ( -9.422394424380274864E-16, 1.000000000000000000, -0.000000000000000000 ) ) ;
#8728 = AXIS2_PLACEMENT_3D ( 'NONE', #5431, #10598, #12862 ) ;
#8729 = DIRECTION ( 'NONE',  ( 0.000000000000000000, 0.000000000000000000, 1.000000000000000000 ) ) ;
#8730 = CARTESIAN_POINT ( 'NONE',  ( 26.62067127263865274, -1.924145975121151140E-15, 23.92684502045323924 ) ) ;
#8731 = DIRECTION ( 'NONE',  ( 0.000000000000000000, 0.000000000000000000, -1.000000000000000000 ) ) ;
#8732 = DIRECTION ( 'NONE',  ( 0.8660254037844387076, 0.4999999999999998890, 0.000000000000000000 ) ) ;
#8733 = CARTESIAN_POINT ( 'NONE',  ( -35.58670980944424400, 5.000000000000000000, 97.50956111919106206 ) ) ;
#8734 = FACE_OUTER_BOUND ( 'NONE', #4611, .T. ) ;
#8735 = AXIS2_PLACEMENT_3D ( 'NONE', #10380, #12717, #12642 ) ;
#8736 = DIRECTION ( 'NONE',  ( 0.000000000000000000, 0.000000000000000000, -1.000000000000000000 ) ) ;
#8737 = EDGE_LOOP ( 'NONE', ( #13241, #13730, #13177 ) ) ;
#8738 = EDGE_LOOP ( 'NONE', ( #11013, #9457, #11800, #8896 ) ) ;
#8739 = CIRCLE ( 'NONE', #1057, 0.6000000000000000888 ) ;
#8740 = DIRECTION ( 'NONE',  ( 0.000000000000000000, 0.000000000000000000, 1.000000000000000000 ) ) ;
#8741 = CARTESIAN_POINT ( 'NONE',  ( -2.381388125886219509, -1.944375000000168052, -2.899558211763606508 ) ) ;
#8742 = VERTEX_POINT ( 'NONE', #1053 ) ;
#8743 = EDGE_CURVE ( 'NONE', #11184, #6866, #6672, .T. ) ;
#8744 = AXIS2_PLACEMENT_3D ( 'NONE', #15305, #3684, #8414 ) ;
#8745 = CARTESIAN_POINT ( 'NONE',  ( -56.52438362643999170, 65.17411849586700612, -150.4984795835770228 ) ) ;
#8746 = VECTOR ( 'NONE', #3192, 1000.000000000000000 ) ;
#8747 = CARTESIAN_POINT ( 'NONE',  ( 2.919796888921922573, -5.104126807837104707, -2.256669152708658643 ) ) ;
#8748 = CARTESIAN_POINT ( 'NONE',  ( -5.196152422706630247, 0.1227504548087275521, -7.569115911492098221E-16 ) ) ;
#8749 = AXIS2_PLACEMENT_3D ( 'NONE', #11638, #11795, #4735 ) ;
#8750 = DIRECTION ( 'NONE',  ( 0.000000000000000000, 0.000000000000000000, 1.000000000000000000 ) ) ;
#8751 = SURFACE_STYLE_USAGE ( .BOTH. , #4023 ) ;
#8752 = DIRECTION ( 'NONE',  ( -1.000000000000000000, -2.622621077317916910E-15, 0.000000000000000000 ) ) ;
#8753 = DIRECTION ( 'NONE',  ( 0.000000000000000000, 0.000000000000000000, 1.000000000000000000 ) ) ;
#8754 = ADVANCED_FACE ( 'NONE', ( #9357 ), #2452, .F. ) ;
#8755 = ORIENTED_EDGE ( 'NONE', *, *, #7580, .T. ) ;
#8756 = CARTESIAN_POINT ( 'NONE',  ( 16.54686605390242349, -0.2715358723599884394, -23.33896727494797929 ) ) ;
#8757 = AXIS2_PLACEMENT_3D ( 'NONE', #5702, #11886, #3667 ) ;
#8758 = VECTOR ( 'NONE', #11242, 1000.000000000000114 ) ;
#8759 = VERTEX_POINT ( 'NONE', #1137 ) ;
#8760 = VERTEX_POINT ( 'NONE', #10672 ) ;
#8761 = ORIENTED_EDGE ( 'NONE', *, *, #4711, .T. ) ;
#8762 = ORIENTED_EDGE ( 'NONE', *, *, #4976, .F. ) ;
#8763 = EDGE_CURVE ( 'NONE', #9085, #12591, #11686, .T. ) ;
#8764 = ORIENTED_EDGE ( 'NONE', *, *, #3544, .F. ) ;
#8765 = CONICAL_SURFACE ( 'NONE', #9182, 3.968749999999992895, 0.7155849933176756661 ) ;
#8766 = CARTESIAN_POINT ( 'NONE',  ( -38.27438362644000591, 60.67411849586700612, -79.49847958357700861 ) ) ;
#8767 = CARTESIAN_POINT ( 'NONE',  ( -3.657957510581538507, -2.116249999999859632, 0.7266254446581354998 ) ) ;
#8768 = EDGE_CURVE ( 'NONE', #4543, #726, #2376, .T. ) ;
#8769 = EDGE_CURVE ( 'NONE', #5984, #7742, #7895, .T. ) ;
#8770 =( LENGTH_UNIT ( ) NAMED_UNIT ( * ) SI_UNIT ( .MILLI., .METRE. ) );
#8771 = CARTESIAN_POINT ( 'NONE',  ( -2.415777803760090325, -4.359374999999756639, -2.941435367455751848 ) ) ;
#8772 = CIRCLE ( 'NONE', #4073, 1.199999999999999734 ) ;
#8773 = CARTESIAN_POINT ( 'NONE',  ( -12.81835358098578403, -12.00000029085423314, -14.73358795631400575 ) ) ;
#8774 = VECTOR ( 'NONE', #1841, 1000.000000000000000 ) ;
#8775 = DIRECTION ( 'NONE',  ( 1.000000000000000000, 0.000000000000000000, 0.000000000000000000 ) ) ;
#8776 = DIRECTION ( 'NONE',  ( -0.08715574274766157981, 1.084202172485503818E-16, 0.9961946980917452121 ) ) ;
#8777 = CARTESIAN_POINT ( 'NONE',  ( -4.293030807686615269, -0.5110219675973943776, 0.2974983986620418630 ) ) ;
#8778 = CARTESIAN_POINT ( 'NONE',  ( -86.77438362644100778, 101.5320169952374414, -147.9984795835769944 ) ) ;
#8779 = FACE_OUTER_BOUND ( 'NONE', #451, .T. ) ;
#8780 = ADVANCED_FACE ( 'NONE', ( #15244 ), #6425, .T. ) ;
#8781 = ORIENTED_EDGE ( 'NONE', *, *, #4895, .T. ) ;
#8782 = DIRECTION ( 'NONE',  ( 1.517216463963902273E-16, -1.000000000000000000, -1.734186353771755353E-15 ) ) ;
#8783 = VERTEX_POINT ( 'NONE', #4790 ) ;
#8784 = EDGE_LOOP ( 'NONE', ( #2475, #14393, #1687 ) ) ;
#8785 = ORIENTED_EDGE ( 'NONE', *, *, #14616, .T. ) ;
#8786 = CARTESIAN_POINT ( 'NONE',  ( -2.488972454571051429, -5.975625000000068354, -2.041081048424583155 ) ) ;
#8787 = VECTOR ( 'NONE', #13340, 1000.000000000000000 ) ;
#8788 = AXIS2_PLACEMENT_3D ( 'NONE', #12031, #8907, #10291 ) ;
#8789 = EDGE_CURVE ( 'NONE', #1628, #15023, #14242, .T. ) ;
#8790 = DIRECTION ( 'NONE',  ( 0.000000000000000000, 0.000000000000000000, -1.000000000000000000 ) ) ;
#8791 = DIRECTION ( 'NONE',  ( -0.000000000000000000, -0.000000000000000000, 1.000000000000000000 ) ) ;
#8792 = CARTESIAN_POINT ( 'NONE',  ( -62.02799568714584666, 110.1741184958670061, -152.4984795835769944 ) ) ;
#8793 = CARTESIAN_POINT ( 'NONE',  ( -88.81638362644000040, 66.35306774555222376, -147.9984795835769944 ) ) ;
#8794 = FACE_OUTER_BOUND ( 'NONE', #5027, .T. ) ;
#8795 = CIRCLE ( 'NONE', #12309, 1.999999999999988010 ) ;
#8796 = CARTESIAN_POINT ( 'NONE',  ( 0.8000000000000175859, 9.500000000000000000, 9.797174393179039389E-17 ) ) ;
#8797 = ORIENTED_EDGE ( 'NONE', *, *, #6056, .F. ) ;
#8798 = VECTOR ( 'NONE', #11334, 1000.000000000000000 ) ;
#8799 = DIRECTION ( 'NONE',  ( 0.000000000000000000, 0.000000000000000000, 1.000000000000000000 ) ) ;
#8800 = VERTEX_POINT ( 'NONE', #10760 ) ;
#8801 = B_SPLINE_SURFACE_WITH_KNOTS ( 'NONE', 1, 3, ( 
 ( #8554, #6329, #12364, #1501, #9064, #8786, #8705, #325, #13302, #5071, #14597, #1575, #11389, #3976, #4341, #5156, #9787, #12634, #14519, #13454, #14948, #8630, #12132, #248, #2816, #9866, #2897, #6405, #1655, #4993, #1725, #3172, #6252, #13378, #12286, #14442, #754, #5513, #413, #11041, #9707, #11117, #3827, #2663, #7409, #2734, #489, #10213, #5224, #9939, #10443, #6906, #11698, #5676, #10371, #12946, #4482, #987, #10297, #3239, #3320, #8136, #1147, #14026, #9204, #8051, #10607, #5740, #15172, #4722, #9288, #11549, #13945, #837, #15329, #2306, #7972, #3400, #12870, #7058, #9366, #2230, #6973, #1062, #12707, #10526, #4650, #2079, #3474, #6829, #13028, #5592, #11777, #9437, #3551, #916, #9663, #56, #10773, #280, #3707, #12094, #210, #5030, #11932, #4955, #6059, #9591, #7210, #8434, #10682, #9747, #9829, #14254, #13179, #1299, #8664, #2540, #14561, #6213, #6289, #2622, #8369, #2460, #7370, #14330, #7444, #12158, #7290, #3943, #12016, #14395, #3784, #5981, #11000, #2387, #14482, #4801, #13112, #1461, #3869, #8596, #7138, #1384, #11857, #132, #6141, #10850, #9515, #369, #4885, #8514, #10921, #13342, #2699, #1532, #5117, #1222, #3636, #11375, #6666, #12241, #4175, #6442, #5340, #6588, #741, #454, #12325, #522, #1914, #5496, #14627, #12399, #10198, #3082, #14931, #8741, #590, #2770, #4012, #13569, #11081, #7523, #1834, #8972, #13487, #1612, #4094, #6366, #14856, #12552, #7817, #2852, #3007, #1759, #8899, #4320, #11150, #13639, #8822, #11301, #1691, #13409, #4244, #5191, #13712, #9902, #7600, #5259, #670, #9976, #14706, #2935, #7676, #6509, #11224, #10054, #14786, #7745, #12473, #5423, #10124, #14009, #10426, #8033, #3385, #8117, #9187, #7037, #2288, #7889, #15154, #2064, #972, #2213, #11760, #11453, #7954, #11531, #12926, #1129, #10275, #12772, #5890, #14090, #10592, #4396, #11608, #13787, #15006, #13930, #6734, #3158, #12851, #4632, #9117, #12621 ),
 ( #1045, #2141, #9350, #6887, #5655, #11677, #13855, #10355, #15315, #3223, #5724, #3456, #15080, #6956, #5802, #4546, #819, #9045, #5574, #4467, #9269, #10507, #1984, #3302, #12691, #6812, #15236, #8188, #896, #2680, #13240, #2520, #4779, #7120, #9497, #8422, #1278, #262, #13164, #13320, #14314, #14234, #1513, #3618, #7270, #8574, #13095, #5966, #6269, #11994, #3693, #2597, #192, #10830, #10982, #10904, #7425, #36, #8353, #6123, #8268, #9728, #14465, #9573, #10750, #4706, #1360, #12144, #9417, #1207, #2446, #7196, #8496, #11916, #6042, #112, #13008, #12077, #14157, #10662, #4864, #4939, #3533, #9648, #2367, #7349, #11840, #14381, #3766, #1442, #6198, #5012, #3847, #5409, #11133, #7803, #12307, #7661, #12382, #3921, #8952, #349, #2987, #8646, #6350, #11204, #13621, #1815, #12532, #1676, #1899, #14611, #7582, #8803, #2747, #4228, #13470, #5240, #14689, #5321, #1740, #4077, #10036, #14772, #505, #13692, #3064, #14539, #6490, #8722, #572, #8883, #6653, #7502, #3991, #2833, #5093, #9807, #1595, #13555, #13391, #10110, #12220, #11064, #2918, #434, #5172, #9956, #9883, #6422, #4159, #11285, #7725, #12453, #6570, #654, #14842, #10493, #5784, #11435, #956, #15066, #6871, #4610, #4382, #2122, #6796, #4530, #10260, #1030, #2199, #11361, #6942, #11660, #9333, #9102, #11514, #11592, #13768, #5710, #13914, #3142, #878, #12608, #12905, #2271, #8098, #14072, #3286, #13991, #8018, #9029, #13843, #9253, #12675, #10409, #9172, #3365, #5557, #12755, #14988, #3442, #8175, #5481, #7875, #729, #15138, #10179, #14911, #4301, #12836, #4455, #6720, #800, #7941, #5641, #10340, #3600, #8556, #11825, #3678, #2582, #8336, #10814, #9636, #2500, #4690, #10893, #9403, #2433, #11975, #3748, #13304, #1259, #3831, #14140, #7181, #8477, #12994, #4995, #4927, #4846, #1191, #3515, #5949, #95, #13081, #7331, #14301, #250, #6025, #10647, #7018, #19, #1344, #9709, #4764, #8248 ) ),
 .UNSPECIFIED., .F., .F., .F.,
 ( 2, 2 ),
 ( 4, 2, 2, 2, 2, 2, 2, 2, 2, 2, 2, 2, 2, 2, 2, 2, 2, 2, 2, 2, 2, 2, 2, 2, 2, 2, 2, 2, 2, 2, 2, 2, 2, 2, 2, 2, 2, 2, 2, 2, 2, 2, 2, 2, 2, 2, 2, 2, 2, 2, 2, 2, 2, 2, 2, 2, 2, 2, 2, 2, 2, 2, 2, 2, 2, 2, 2, 2, 2, 2, 2, 2, 2, 2, 2, 2, 2, 2, 2, 2, 2, 2, 2, 2, 2, 2, 2, 2, 2, 2, 2, 2, 2, 2, 2, 2, 2, 2, 2, 2, 2, 2, 2, 2, 2, 2, 2, 2, 2, 2, 2, 2, 2, 2, 2, 2, 2, 2, 2, 2, 2, 2, 2, 2, 2, 2, 2, 2, 4 ),
 ( 0.000000000000000000, 1.000000000000000000 ),
 ( 0.000000000000000000, 0.007812500000000000000, 0.01562500000000000000, 0.02343750000000000000, 0.03125000000000000000, 0.03906250000000000000, 0.04687500000000000000, 0.05468750000000000000, 0.06250000000000000000, 0.07031250000000000000, 0.07812500000000000000, 0.08593750000000000000, 0.09375000000000000000, 0.1015625000000000000, 0.1093750000000000000, 0.1171875000000000000, 0.1250000000000000000, 0.1328125000000000000, 0.1406250000000000000, 0.1484375000000000000, 0.1562500000000000000, 0.1640625000000000000, 0.1718750000000000000, 0.1796875000000000000, 0.1875000000000000000, 0.1953125000000000000, 0.2031250000000000000, 0.2109375000000000000, 0.2187500000000000000, 0.2265625000000000000, 0.2343750000000000000, 0.2421875000000000000, 0.2500000000000000000, 0.2578125000000000000, 0.2656250000000000000, 0.2734375000000000000, 0.2812500000000000000, 0.2890625000000000000, 0.2968750000000000000, 0.3046875000000000000, 0.3125000000000000000, 0.3203125000000000000, 0.3281250000000000000, 0.3359375000000000000, 0.3437500000000000000, 0.3515625000000000000, 0.3593750000000000000, 0.3671875000000000000, 0.3750000000000000000, 0.3828125000000000000, 0.3906250000000000000, 0.3984375000000000000, 0.4062500000000000000, 0.4140625000000000000, 0.4218750000000000000, 0.4296875000000000000, 0.4375000000000000000, 0.4453125000000000000, 0.4531250000000000000, 0.4609375000000000000, 0.4687500000000000000, 0.4765625000000000000, 0.4843750000000000000, 0.4921875000000000000, 0.5000000000000000000, 0.5078125000000000000, 0.5156250000000000000, 0.5234375000000000000, 0.5312500000000000000, 0.5390625000000000000, 0.5468750000000000000, 0.5546875000000000000, 0.5625000000000000000, 0.5703125000000000000, 0.5781250000000000000, 0.5859375000000000000, 0.5937500000000000000, 0.6015625000000000000, 0.6093750000000000000, 0.6171875000000000000, 0.6250000000000000000, 0.6328125000000000000, 0.6406250000000000000, 0.6484375000000000000, 0.6562500000000000000, 0.6640625000000000000, 0.6718750000000000000, 0.6796875000000000000, 0.6875000000000000000, 0.6953125000000000000, 0.7031250000000000000, 0.7109375000000000000, 0.7187500000000000000, 0.7265625000000000000, 0.7343750000000000000, 0.7421875000000000000, 0.7500000000000000000, 0.7578125000000000000, 0.7656250000000000000, 0.7734375000000000000, 0.7812500000000000000, 0.7890625000000000000, 0.7968750000000000000, 0.8046875000000000000, 0.8125000000000000000, 0.8203125000000000000, 0.8281250000000000000, 0.8359375000000000000, 0.8437500000000000000, 0.8515625000000000000, 0.8593750000000000000, 0.8671875000000000000, 0.8750000000000000000, 0.8828125000000000000, 0.8906250000000000000, 0.8984375000000000000, 0.9062500000000000000, 0.9140625000000000000, 0.9218750000000000000, 0.9296875000000000000, 0.9375000000000000000, 0.9453125000000000000, 0.9531250000000000000, 0.9609375000000000000, 0.9687500000000000000, 0.9765625000000000000, 0.9843750000000000000, 0.9921875000000000000, 1.000000000000000000 ),
 .UNSPECIFIED. ) ;
#8802 = LINE ( 'NONE', #3920, #138 ) ;
#8803 = CARTESIAN_POINT ( 'NONE',  ( 2.541707380700019225, -2.859374999999939160, 3.094782911937220771 ) ) ;
#8804 = ORIENTED_EDGE ( 'NONE', *, *, #1666, .T. ) ;
#8805 = STYLED_ITEM ( 'NONE', ( #11676 ), #330 ) ;
#8806 = TOROIDAL_SURFACE ( 'NONE', #10794, 2.400000000000000355, 0.6000000000000000888 ) ;
#8807 = TOROIDAL_SURFACE ( 'NONE', #13284, 2.400000000000000355, 0.6000000000000000888 ) ;
#8808 = CARTESIAN_POINT ( 'NONE',  ( -69.77438362644001302, 74.17411849586699191, -29.37106258560738681 ) ) ;
#8809 = CARTESIAN_POINT ( 'NONE',  ( -13.41835358098578723, -11.40000029085424416, 0.2664120436859911956 ) ) ;
#8810 = CARTESIAN_POINT ( 'NONE',  ( -13.41835358098578723, -11.40000029085424238, 0.2664120436859911956 ) ) ;
#8811 = CARTESIAN_POINT ( 'NONE',  ( 0.000000000000000000, 0.000000000000000000, 0.000000000000000000 ) ) ;
#8812 = CARTESIAN_POINT ( 'NONE',  ( -69.77438362644001302, 82.17411849586700612, -44.99847958358749622 ) ) ;
#8813 = DIRECTION ( 'NONE',  ( -0.7071067811865474617, 8.659560562354921765E-17, 0.7071067811865474617 ) ) ;
#8814 = FACE_OUTER_BOUND ( 'NONE', #73, .T. ) ;
#8815 = DIRECTION ( 'NONE',  ( 0.000000000000000000, 0.000000000000000000, 1.000000000000000000 ) ) ;
#8816 = AXIS2_PLACEMENT_3D ( 'NONE', #10345, #15072, #14995 ) ;
#8817 = CIRCLE ( 'NONE', #10289, 0.6000000000000000888 ) ;
#8818 = ORIENTED_EDGE ( 'NONE', *, *, #11679, .F. ) ;
#8819 = ADVANCED_FACE ( 'NONE', ( #121 ), #3683, .F. ) ;
#8820 = VERTEX_POINT ( 'NONE', #10990 ) ;
#8821 = CARTESIAN_POINT ( 'NONE',  ( -86.77438362643999881, 67.53201699523744139, -147.9984795835769944 ) ) ;
#8822 = CARTESIAN_POINT ( 'NONE',  ( 1.801006600569702520, -1.413124999999811449, 3.371562913404279271 ) ) ;
#8823 = VERTEX_POINT ( 'NONE', #3930 ) ;
#8824 = AXIS2_PLACEMENT_3D ( 'NONE', #14116, #7852, #6694 ) ;
#8825 = CARTESIAN_POINT ( 'NONE',  ( -86.77438362643999881, 67.53201699523744139, -147.9984795835769944 ) ) ;
#8826 = CIRCLE ( 'NONE', #7604, 0.2000000000000057288 ) ;
#8827 = AXIS2_PLACEMENT_3D ( 'NONE', #15052, #9013, #12737 ) ;
#8828 = LINE ( 'NONE', #11155, #180 ) ;
#8829 = CARTESIAN_POINT ( 'NONE',  ( 2.598076211353314235, 0.1227504548087474667, -4.499999999999999112 ) ) ;
#8830 = CARTESIAN_POINT ( 'NONE',  ( 3.405785683274218378, -0.4995676945082505038, -2.189026399521772248 ) ) ;
#8831 = CARTESIAN_POINT ( 'NONE',  ( -57.27438362644000591, 99.17411849586700612, -86.49847958357699440 ) ) ;
#8832 = CARTESIAN_POINT ( 'NONE',  ( 12.30141533273650900, -8.891480818932939924E-16, 55.44770860939965473 ) ) ;
#8833 = EDGE_CURVE ( 'NONE', #541, #7520, #13330, .T. ) ;
#8834 = LINE ( 'NONE', #14720, #14718 ) ;
#8835 = VERTEX_POINT ( 'NONE', #7358 ) ;
#8836 = CYLINDRICAL_SURFACE ( 'NONE', #6556, 1.000000000000000000 ) ;
#8837 = TOROIDAL_SURFACE ( 'NONE', #2389, 3.299999999999470024, 0.2000000000005275058 ) ;
#8838 = EDGE_CURVE ( 'NONE', #9550, #14746, #1604, .T. ) ;
#8839 = EDGE_LOOP ( 'NONE', ( #536, #12837, #14390, #2405 ) ) ;
#8840 = VECTOR ( 'NONE', #7145, 1000.000000000000000 ) ;
#8841 = ORIENTED_EDGE ( 'NONE', *, *, #14642, .F. ) ;
#8842 = ORIENTED_EDGE ( 'NONE', *, *, #3905, .F. ) ;
#8843 = ORIENTED_EDGE ( 'NONE', *, *, #3425, .T. ) ;
#8844 = ORIENTED_EDGE ( 'NONE', *, *, #12384, .F. ) ;
#8845 = DIRECTION ( 'NONE',  ( 0.000000000000000000, 0.000000000000000000, 1.000000000000000000 ) ) ;
#8846 = DIRECTION ( 'NONE',  ( -2.551930889570660354E-15, 1.000000000000000000, 0.000000000000000000 ) ) ;
#8847 = AXIS2_PLACEMENT_3D ( 'NONE', #4604, #950, #3359 ) ;
#8848 = CARTESIAN_POINT ( 'NONE',  ( 0.0009972298945177876170, -4.250000000000088818, -3.820821809411817149 ) ) ;
#8849 = CARTESIAN_POINT ( 'NONE',  ( -16.75000000000000355, -0.2715193793361416197, 22.01281590054916748 ) ) ;
#8850 = DIRECTION ( 'NONE',  ( 1.000000000000000000, 0.000000000000000000, 0.000000000000000000 ) ) ;
#8851 = CARTESIAN_POINT ( 'NONE',  ( -46.58670980944423690, 0.000000000000000000, 135.5095611191910621 ) ) ;
#8852 = CARTESIAN_POINT ( 'NONE',  ( -3.873284713637146215, -1.437499999999919620, -1.605572741981209139 ) ) ;
#8853 = DIRECTION ( 'NONE',  ( -0.8660254037844387076, -0.4999999999999998890, 0.000000000000000000 ) ) ;
#8854 = EDGE_CURVE ( 'NONE', #2626, #8823, #7423, .T. ) ;
#8855 = LINE ( 'NONE', #11715, #154 ) ;
#8856 = CARTESIAN_POINT ( 'NONE',  ( -76.26311196519618818, 67.29799558322736175, -83.44847958357698303 ) ) ;
#8857 = VERTEX_POINT ( 'NONE', #1682 ) ;
#8858 = CARTESIAN_POINT ( 'NONE',  ( -77.52077156573416516, 59.67411849586701322, -15.85886927678779834 ) ) ;
#8859 = EDGE_CURVE ( 'NONE', #10111, #14573, #11616, .T. ) ;
#8860 = ORIENTED_EDGE ( 'NONE', *, *, #2428, .F. ) ;
#8861 = ORIENTED_EDGE ( 'NONE', *, *, #9810, .T. ) ;
#8862 = ORIENTED_EDGE ( 'NONE', *, *, #9522, .F. ) ;
#8863 = UNCERTAINTY_MEASURE_WITH_UNIT (LENGTH_MEASURE( 1.000000000000000082E-05 ), #4863, 'distance_accuracy_value', 'NONE');
#8864 = AXIS2_PLACEMENT_3D ( 'NONE', #2420, #2653, #9694 ) ;
#8865 = DIRECTION ( 'NONE',  ( 0.000000000000000000, 0.000000000000000000, -1.000000000000000000 ) ) ;
#8866 = CARTESIAN_POINT ( 'NONE',  ( 3.270563417710622645, -5.585000000000047038, 0.0008246681304769601546 ) ) ;
#8867 = EDGE_CURVE ( 'NONE', #4176, #11511, #718, .T. ) ;
#8868 = DIRECTION ( 'NONE',  ( 1.000000000000000000, 2.551930889570660354E-15, 0.000000000000000000 ) ) ;
#8869 = ADVANCED_FACE ( 'NONE', ( #5330 ), #12390, .F. ) ;
#8870 = PLANE ( 'NONE',  #8211 ) ;
#8871 = CARTESIAN_POINT ( 'NONE',  ( 15.50000000000000000, -0.2038245569916610489, -23.94337567297399971 ) ) ;
#8872 = DIRECTION ( 'NONE',  ( 0.000000000000000000, 1.000000000000000000, 0.000000000000000000 ) ) ;
#8873 = CARTESIAN_POINT ( 'NONE',  ( -71.12250604111743257, 75.17411849586699191, -44.11946707556889180 ) ) ;
#8874 = EDGE_CURVE ( 'NONE', #7247, #11128, #8895, .T. ) ;
#8875 = CARTESIAN_POINT ( 'NONE',  ( 1.614039610742502573, -4.413124999999970655, 3.021508266705727586 ) ) ;
#8876 = ORIENTED_EDGE ( 'NONE', *, *, #15082, .T. ) ;
#8877 = FACE_BOUND ( 'NONE', #2576, .T. ) ;
#8878 = EDGE_CURVE ( 'NONE', #8760, #8497, #14832, .T. ) ;
#8879 = EDGE_CURVE ( 'NONE', #15166, #8152, #15320, .T. ) ;
#8880 = ITEM_DEFINED_TRANSFORMATION ( 'NONE', 'NONE', #12206,  #285 ) ;
#8881 = EDGE_LOOP ( 'NONE', ( #3083, #12590, #3283, #10404 ) ) ;
#8882 = DIRECTION ( 'NONE',  ( 1.001323786595528197E-17, -1.000000000000000000, -5.421010862427522786E-17 ) ) ;
#8883 = CARTESIAN_POINT ( 'NONE',  ( -3.752022838101215285, -2.437499999999895195, -1.552542887664947635 ) ) ;
#8884 = ORIENTED_EDGE ( 'NONE', *, *, #5955, .F. ) ;
#8885 = CARTESIAN_POINT ( 'NONE',  ( 0.3822547408368546229, -3.764838562373000741, 3.866615621364059230 ) ) ;
#8886 = VECTOR ( 'NONE', #12248, 1000.000000000000000 ) ;
#8887 = CARTESIAN_POINT ( 'NONE',  ( -13.41835358098578723, -11.40000029085424416, 0.2664120436859911956 ) ) ;
#8888 = DIRECTION ( 'NONE',  ( 0.000000000000000000, 1.000000000000000000, 0.000000000000000000 ) ) ;
#8889 = CARTESIAN_POINT ( 'NONE',  ( 0.8667276783653437011, 1.850460790996585685E-15, -4.499999999999999112 ) ) ;
#8890 = CARTESIAN_POINT ( 'NONE',  ( -52.77438362644000591, 65.17411849586700612, -152.4984795835769944 ) ) ;
#8891 = DIRECTION ( 'NONE',  ( 0.7071067811865474617, 0.000000000000000000, 0.7071067811865474617 ) ) ;
#8892 = LINE ( 'NONE', #12463, #10050 ) ;
#8893 = PLANE ( 'NONE',  #10573 ) ;
#8894 = CARTESIAN_POINT ( 'NONE',  ( -35.58670980944424400, 5.000000000000000000, 99.29549861919106490 ) ) ;
#8895 = CIRCLE ( 'NONE', #7672, 4.500000000000000888 ) ;
#8896 = ORIENTED_EDGE ( 'NONE', *, *, #5960, .F. ) ;
#8897 = EDGE_LOOP ( 'NONE', ( #12671, #10663, #6649, #1089, #9290, #54 ) ) ;
#8898 = CARTESIAN_POINT ( 'NONE',  ( -71.13655333277267800, 74.17411849586700612, -58.99847958357691624 ) ) ;
#8899 = CARTESIAN_POINT ( 'NONE',  ( 3.359686712366170447, -1.506874999999983755, 1.796916873358725963 ) ) ;
#8900 = ORIENTED_EDGE ( 'NONE', *, *, #5170, .F. ) ;
#8901 = PLANE ( 'NONE',  #1267 ) ;
#8902 = DIRECTION ( 'NONE',  ( 0.000000000000000000, 0.000000000000000000, 1.000000000000000000 ) ) ;
#8903 = PLANE ( 'NONE',  #11255 ) ;
#8904 = CARTESIAN_POINT ( 'NONE',  ( -4.244864575696460918, -0.4995676945082702658, -0.6400435777867373721 ) ) ;
#8905 = DIRECTION ( 'NONE',  ( 0.000000000000000000, 0.000000000000000000, 1.000000000000000000 ) ) ;
#8906 = CARTESIAN_POINT ( 'NONE',  ( -56.85838362644099675, 99.17411849586700612, -147.9984795835769944 ) ) ;
#8907 = DIRECTION ( 'NONE',  ( 1.000000000000000000, 0.000000000000000000, -0.000000000000000000 ) ) ;
#8908 = ORIENTED_EDGE ( 'NONE', *, *, #9703, .F. ) ;
#8909 = DIRECTION ( 'NONE',  ( 0.000000000000000000, -0.000000000000000000, 1.000000000000000000 ) ) ;
#8910 = EDGE_LOOP ( 'NONE', ( #12971, #7619, #10525, #3746, #7818, #8781, #9129, #1145, #14073, #20 ) ) ;
#8911 = PRODUCT_DEFINITION_FORMATION_WITH_SPECIFIED_SOURCE ( 'ANY', '', #5218, .NOT_KNOWN. ) ;
#8912 = ORIENTED_EDGE ( 'NONE', *, *, #5920, .F. ) ;
#8913 = ORIENTED_EDGE ( 'NONE', *, *, #3651, .T. ) ;
#8914 = ORIENTED_EDGE ( 'NONE', *, *, #10492, .F. ) ;
#8915 = EDGE_LOOP ( 'NONE', ( #12605, #1673, #2330 ) ) ;
#8916 = CARTESIAN_POINT ( 'NONE',  ( 2.551069250243800379, -5.874213562372941233, 2.549185564325499698 ) ) ;
#8917 = EDGE_CURVE ( 'NONE', #12550, #14746, #6357, .T. ) ;
#8918 = CARTESIAN_POINT ( 'NONE',  ( -0.7236788045118704993, -2.303749999999964437, 3.633254187536902435 ) ) ;
#8919 = DIRECTION ( 'NONE',  ( 0.000000000000000000, 0.000000000000000000, -1.000000000000000000 ) ) ;
#8920 = CARTESIAN_POINT ( 'NONE',  ( 3.568675334318531345, -3.937499999999699796, 1.476665218992084139 ) ) ;
#8921 = CARTESIAN_POINT ( 'NONE',  ( 15.50000000000000000, -1.037157890325000054, -22.50000000000000000 ) ) ;
#8922 = EDGE_CURVE ( 'NONE', #11316, #587, #2202, .T. ) ;
#8923 = DIRECTION ( 'NONE',  ( -1.740799290094577062E-15, -1.000000000000000000, -6.292789498690070142E-18 ) ) ;
#8924 = CARTESIAN_POINT ( 'NONE',  ( -52.77438362644100067, 99.17411849586700612, -149.9984795835770228 ) ) ;
#8925 = CARTESIAN_POINT ( 'NONE',  ( -3.468190155366909888, -1.593749999999917621, 2.319185894079683230 ) ) ;
#8926 = DIRECTION ( 'NONE',  ( 0.8660254037844383745, -0.5000000000000003331, 0.000000000000000000 ) ) ;
#8927 = CARTESIAN_POINT ( 'NONE',  ( -60.52799568714584666, 60.67411849586701322, -79.59847958357700293 ) ) ;
#8928 = CARTESIAN_POINT ( 'NONE',  ( -51.75338362644099277, 100.9425423703948326, -147.9984795835769944 ) ) ;
#8929 = EDGE_LOOP ( 'NONE', ( #13869, #13805, #4481, #2021, #2250, #6416 ) ) ;
#8930 = CARTESIAN_POINT ( 'NONE',  ( -82.52438362644100778, 99.17411849586700612, -145.4984795835769944 ) ) ;
#8931 = VERTEX_POINT ( 'NONE', #9738 ) ;
#8932 = ORIENTED_EDGE ( 'NONE', *, *, #2972, .T. ) ;
#8933 = ORIENTED_EDGE ( 'NONE', *, *, #2039, .T. ) ;
#8934 = CARTESIAN_POINT ( 'NONE',  ( 17.18164641901421419, -11.40000029085424238, 0.8664120436859875651 ) ) ;
#8935 = EDGE_CURVE ( 'NONE', #11838, #15131, #582, .T. ) ;
#8936 = CARTESIAN_POINT ( 'NONE',  ( -2.129528971937844517, -4.944374999999755715, -2.592863122870853410 ) ) ;
#8937 = DIRECTION ( 'NONE',  ( 0.000000000000000000, 0.000000000000000000, -1.000000000000000000 ) ) ;
#8938 = DIRECTION ( 'NONE',  ( 0.000000000000000000, -1.000000000000000000, -4.336808689942017736E-16 ) ) ;
#8939 = DIRECTION ( 'NONE',  ( 0.000000000000000000, 0.000000000000000000, -1.000000000000000000 ) ) ;
#8940 = CIRCLE ( 'NONE', #11420, 0.5999999999999998668 ) ;
#8941 = DIRECTION ( 'NONE',  ( 0.000000000000000000, 1.000000000000000000, 0.000000000000000000 ) ) ;
#8942 = CARTESIAN_POINT ( 'NONE',  ( -1.414968154826750535, -0.4995676945082624387, 3.878355829113487641 ) ) ;
#8943 = VECTOR ( 'NONE', #12929, 1000.000000000000000 ) ;
#8944 = FACE_OUTER_BOUND ( 'NONE', #10847, .T. ) ;
#8945 = ORIENTED_EDGE ( 'NONE', *, *, #2913, .T. ) ;
#8946 = DIRECTION ( 'NONE',  ( 0.000000000000000000, 0.000000000000000000, 1.000000000000000000 ) ) ;
#8947 = VERTEX_POINT ( 'NONE', #510 ) ;
#8948 = EDGE_CURVE ( 'NONE', #3237, #11860, #9966, .T. ) ;
#8949 = FACE_BOUND ( 'NONE', #14133, .T. ) ;
#8950 = ORIENTED_EDGE ( 'NONE', *, *, #6219, .T. ) ;
#8951 = VECTOR ( 'NONE', #13473, 1000.000000000000000 ) ;
#8952 = CARTESIAN_POINT ( 'NONE',  ( 1.869272562217232592, -3.171875000000011990, -3.494952631674145938 ) ) ;
#8953 = ORIENTED_EDGE ( 'NONE', *, *, #12764, .T. ) ;
#8954 = ADVANCED_FACE ( 'NONE', ( #6431 ), #2608, .T. ) ;
#8955 = VECTOR ( 'NONE', #14070, 1000.000000000000000 ) ;
#8956 = DIRECTION ( 'NONE',  ( 0.000000000000000000, 0.000000000000000000, 1.000000000000000000 ) ) ;
#8957 = ADVANCED_FACE ( 'NONE', ( #14474 ), #6436, .T. ) ;
#8958 = DIRECTION ( 'NONE',  ( 1.000000000000000000, 0.000000000000000000, 0.000000000000000000 ) ) ;
#8959 = EDGE_CURVE ( 'NONE', #11131, #12773, #3858, .T. ) ;
#8960 = DIRECTION ( 'NONE',  ( 0.000000000000000000, 0.000000000000000000, 1.000000000000000000 ) ) ;
#8961 = AXIS2_PLACEMENT_3D ( 'NONE', #1195, #1431, #2586 ) ;
#8962 = LINE ( 'NONE', #7883, #6684 ) ;
#8963 = CARTESIAN_POINT ( 'NONE',  ( 1.555132164185506927, 2.118440305037800009, 4.500000000000001776 ) ) ;
#8964 = DIRECTION ( 'NONE',  ( 0.000000000000000000, 0.5000000000000189848, 0.8660254037844277164 ) ) ;
#8965 = DIRECTION ( 'NONE',  ( -1.000000000000000000, 0.000000000000000000, 0.000000000000000000 ) ) ;
#8966 = CARTESIAN_POINT ( 'NONE',  ( -84.02438362643999881, 99.17411849586700612, -145.4984795835769944 ) ) ;
#8967 = ADVANCED_FACE ( 'NONE', ( #12152 ), #1522, .F. ) ;
#8968 = AXIS2_PLACEMENT_3D ( 'NONE', #1925, #749, #10207 ) ;
#8969 = CARTESIAN_POINT ( 'NONE',  ( 0.000000000000000000, 0.000000000000000000, 0.000000000000000000 ) ) ;
#8970 = ORIENTED_EDGE ( 'NONE', *, *, #2329, .T. ) ;
#8971 = FACE_OUTER_BOUND ( 'NONE', #3469, .T. ) ;
#8972 = CARTESIAN_POINT ( 'NONE',  ( 1.779210140229175563, -1.756874999999983755, -3.331607052712223016 ) ) ;
#8973 = ORIENTED_EDGE ( 'NONE', *, *, #1996, .T. ) ;
#8974 = EDGE_CURVE ( 'NONE', #14328, #12810, #12859, .T. ) ;
#8975 = CARTESIAN_POINT ( 'NONE',  ( -96.77438362643999881, 110.1741184958670061, -152.4984795835769944 ) ) ;
#8976 = AXIS2_PLACEMENT_3D ( 'NONE', #13852, #15311, #12768 ) ;
#8977 = DIRECTION ( 'NONE',  ( -0.9961946980917453232, 0.000000000000000000, -0.08715574274766051122 ) ) ;
#8978 = CARTESIAN_POINT ( 'NONE',  ( 57.41329019055577021, 2.488961461112888074, 129.5095611191910621 ) ) ;
#8979 = CARTESIAN_POINT ( 'NONE',  ( 22.33311828159035528, 3.654316742536409812, 0.2664120436859910290 ) ) ;
#8980 = CARTESIAN_POINT ( 'NONE',  ( 17.10023064866893350, 11.27418174095661030, 0.2691555834469856467 ) ) ;
#8981 = VERTEX_POINT ( 'NONE', #4166 ) ;
#8982 = CARTESIAN_POINT ( 'NONE',  ( 16.75000000000000000, -0.2038245569916320166, -23.22168783648699986 ) ) ;
#8983 = ORIENTED_EDGE ( 'NONE', *, *, #10152, .F. ) ;
#8984 = VERTEX_POINT ( 'NONE', #12615 ) ;
#8985 = VERTEX_POINT ( 'NONE', #4235 ) ;
#8986 = VERTEX_POINT ( 'NONE', #2133 ) ;
#8987 = AXIS2_PLACEMENT_3D ( 'NONE', #12119, #236, #1487 ) ;
#8988 = CIRCLE ( 'NONE', #10217, 2.400000000000001243 ) ;
#8989 = ORIENTED_EDGE ( 'NONE', *, *, #15004, .F. ) ;
#8990 = CARTESIAN_POINT ( 'NONE',  ( -84.07438362643999596, 65.17411849586700612, -145.4984795835769944 ) ) ;
#8991 = CARTESIAN_POINT ( 'NONE',  ( 2.769370807496521980, -0.7100000000000333822, -2.767918543042355850 ) ) ;
#8992 = AXIS2_PLACEMENT_3D ( 'NONE', #6205, #8360, #6052 ) ;
#8993 = CARTESIAN_POINT ( 'NONE',  ( -52.77438362644000591, 65.17411849586700612, -86.49847958357699440 ) ) ;
#8994 = DIRECTION ( 'NONE',  ( 1.000000000000000000, 0.000000000000000000, 0.000000000000000000 ) ) ;
#8995 = CARTESIAN_POINT ( 'NONE',  ( -52.77438362644000591, 65.17411849586700612, -145.4984795835769660 ) ) ;
#8996 = CARTESIAN_POINT ( 'NONE',  ( -13.41835358098578723, -11.40000029085423705, -8.183940086454239093 ) ) ;
#8997 = CARTESIAN_POINT ( 'NONE',  ( 3.738955316585249822, -1.078124999999896527, -2.000248979885406619 ) ) ;
#8998 = CARTESIAN_POINT ( 'NONE',  ( -15.50000000000000000, -1.037157890325000054, -22.50000000000000000 ) ) ;
#8999 = CONICAL_SURFACE ( 'NONE', #10988, 3.250000000000015987, 0.4363323129985828275 ) ;
#9000 = CARTESIAN_POINT ( 'NONE',  ( 57.41329019055577021, 5.000000000000000000, 97.50956111919106206 ) ) ;
#9001 = VECTOR ( 'NONE', #9744, 1000.000000000000000 ) ;
#9002 = CARTESIAN_POINT ( 'NONE',  ( 17.23697745638123280, -3.616872831399570831, -0.03314156585704653574 ) ) ;
#9003 = ORIENTED_EDGE ( 'NONE', *, *, #11240, .T. ) ;
#9004 = DIRECTION ( 'NONE',  ( 1.000000000000000000, 0.000000000000000000, 0.000000000000000000 ) ) ;
#9005 = ORIENTED_EDGE ( 'NONE', *, *, #8668, .F. ) ;
#9006 = AXIS2_PLACEMENT_3D ( 'NONE', #2964, #2326, #68 ) ;
#9007 = ORIENTED_EDGE ( 'NONE', *, *, #14333, .F. ) ;
#9008 = EDGE_LOOP ( 'NONE', ( #3099, #6865, #6975, #9827 ) ) ;
#9009 = ADVANCED_FACE ( 'NONE', ( #1907 ), #10189, .T. ) ;
#9010 = CARTESIAN_POINT ( 'NONE',  ( 15.50000000000000000, -0.2038245569916604938, 23.94337567297399971 ) ) ;
#9011 = AXIS2_PLACEMENT_3D ( 'NONE', #4932, #497, #6414 ) ;
#9012 = CIRCLE ( 'NONE', #10006, 16.00000000000000000 ) ;
#9013 = DIRECTION ( 'NONE',  ( 1.000000000000000000, -1.287488025362404182E-15, 0.000000000000000000 ) ) ;
#9014 = LINE ( 'NONE', #10326, #13194 ) ;
#9015 = LINE ( 'NONE', #3128, #1648 ) ;
#9016 = DIRECTION ( 'NONE',  ( -0.000000000000000000, 0.000000000000000000, -1.000000000000000000 ) ) ;
#9017 = DIRECTION ( 'NONE',  ( 0.000000000000000000, -0.000000000000000000, -1.000000000000000000 ) ) ;
#9018 = DIRECTION ( 'NONE',  ( -0.08715574274766131613, 0.000000000000000000, 0.9961946980917453232 ) ) ;
#9019 = CARTESIAN_POINT ( 'NONE',  ( 2.619799856955864925, -4.694374999999869402, -2.148899555557211904 ) ) ;
#9020 = ORIENTED_EDGE ( 'NONE', *, *, #14548, .T. ) ;
#9021 = DIRECTION ( 'NONE',  ( 0.000000000000000000, 0.000000000000000000, -1.000000000000000000 ) ) ;
#9022 = AXIS2_PLACEMENT_3D ( 'NONE', #5116, #1611, #520 ) ;
#9023 = CIRCLE ( 'NONE', #14956, 2.500000000000002220 ) ;
#9024 = EDGE_CURVE ( 'NONE', #14169, #12927, #14779, .T. ) ;
#9025 = VECTOR ( 'NONE', #2707, 1000.000000000000000 ) ;
#9026 = ORIENTED_EDGE ( 'NONE', *, *, #11431, .F. ) ;
#9027 = ORIENTED_EDGE ( 'NONE', *, *, #6851, .T. ) ;
#9028 = EDGE_CURVE ( 'NONE', #8647, #3871, #1830, .T. ) ;
#9029 = CARTESIAN_POINT ( 'NONE',  ( 4.164680137118252468, -1.031249999999941602, -0.8299691317567963189 ) ) ;
#9030 = ORIENTED_EDGE ( 'NONE', *, *, #3940, .F. ) ;
#9031 = DIRECTION ( 'NONE',  ( 0.000000000000000000, 0.000000000000000000, 1.000000000000000000 ) ) ;
#9032 = CIRCLE ( 'NONE', #11763, 0.5999999999999998668 ) ;
#9033 = PLANE ( 'NONE',  #140 ) ;
#9034 = DIRECTION ( 'NONE',  ( 0.000000000000000000, 0.000000000000000000, 1.000000000000000000 ) ) ;
#9035 = CARTESIAN_POINT ( 'NONE',  ( -4.435020996998821019, 11.99999970914572778, 69.03723529703218276 ) ) ;
#9036 = PLANE ( 'NONE',  #6296 ) ;
#9037 = DIRECTION ( 'NONE',  ( -1.000000000000000000, 0.000000000000000000, 0.000000000000000000 ) ) ;
#9038 = DIRECTION ( 'NONE',  ( 0.000000000000000000, 0.000000000000000000, 1.000000000000000000 ) ) ;
#9039 = EDGE_CURVE ( 'NONE', #13360, #12431, #2996, .T. ) ;
#9040 = DIRECTION ( 'NONE',  ( 1.000000000000000000, 0.000000000000000000, 0.000000000000000000 ) ) ;
#9041 =( GEOMETRIC_REPRESENTATION_CONTEXT ( 3 ) GLOBAL_UNCERTAINTY_ASSIGNED_CONTEXT ( ( #8863 ) ) GLOBAL_UNIT_ASSIGNED_CONTEXT ( ( #4863, #9496, #13094 ) ) REPRESENTATION_CONTEXT ( 'NONE', 'WORKASPACE' ) );
#9042 = ORIENTED_EDGE ( 'NONE', *, *, #14564, .T. ) ;
#9043 = EDGE_CURVE ( 'NONE', #11817, #7059, #8962, .T. ) ;
#9044 = VECTOR ( 'NONE', #10306, 1000.000000000000000 ) ;
#9045 = CARTESIAN_POINT ( 'NONE',  ( 2.864761595209854406, -5.109375000000294875, -2.352813015294751953 ) ) ;
#9046 = ORIENTED_EDGE ( 'NONE', *, *, #8538, .F. ) ;
#9047 = VECTOR ( 'NONE', #4814, 1000.000000000000000 ) ;
#9048 = ADVANCED_BREP_SHAPE_REPRESENTATION ( '', ( #385, #285 ), #1033 ) ;
#9049 = ADVANCED_FACE ( 'NONE', ( #4311 ), #13776, .F. ) ;
#9050 = DIRECTION ( 'NONE',  ( 0.000000000000000000, 0.000000000000000000, -1.000000000000000000 ) ) ;
#9051 = FACE_OUTER_BOUND ( 'NONE', #2097, .T. ) ;
#9052 = AXIS2_PLACEMENT_3D ( 'NONE', #11596, #13996, #733 ) ;
#9053 = CARTESIAN_POINT ( 'NONE',  ( -52.77438362643999881, 65.17411849586700612, -147.9984795835769944 ) ) ;
#9054 = CARTESIAN_POINT ( 'NONE',  ( -62.02799568714584666, 110.1741184958670061, -15.85886927678779834 ) ) ;
#9055 = CIRCLE ( 'NONE', #871, 1.785937500000001066 ) ;
#9056 = EDGE_CURVE ( 'NONE', #5926, #6810, #216, .T. ) ;
#9057 = FACE_OUTER_BOUND ( 'NONE', #2264, .T. ) ;
#9058 = ORIENTED_EDGE ( 'NONE', *, *, #1858, .F. ) ;
#9059 = DIRECTION ( 'NONE',  ( 0.000000000000000000, 1.000000000000000000, 0.000000000000000000 ) ) ;
#9060 = VERTEX_POINT ( 'NONE', #11293 ) ;
#9061 = EDGE_CURVE ( 'NONE', #1528, #7246, #1467, .T. ) ;
#9062 = ORIENTED_EDGE ( 'NONE', *, *, #15300, .T. ) ;
#9063 = ADVANCED_FACE ( 'NONE', ( #5415 ), #10116, .F. ) ;
#9064 = CARTESIAN_POINT ( 'NONE',  ( -2.834780744084784754, -6.006874999999924469, -1.516137112471814818 ) ) ;
#9065 = ORIENTED_EDGE ( 'NONE', *, *, #10730, .T. ) ;
#9066 = VECTOR ( 'NONE', #13403, 1000.000000000000114 ) ;
#9067 = ORIENTED_EDGE ( 'NONE', *, *, #13046, .F. ) ;
#9068 = VERTEX_POINT ( 'NONE', #11445 ) ;
#9069 = AXIS2_PLACEMENT_3D ( 'NONE', #12121, #5144, #8619 ) ;
#9070 = CARTESIAN_POINT ( 'NONE',  ( 1.382436512939505757, -5.811713562372810671, 3.339933979889968541 ) ) ;
#9071 = CARTESIAN_POINT ( 'NONE',  ( -3.204583014436136690, -1.178749999999988640, 2.140022251743640691 ) ) ;
#9072 = FACE_OUTER_BOUND ( 'NONE', #14065, .T. ) ;
#9073 = CARTESIAN_POINT ( 'NONE',  ( -3.121978066431621901, -2.609375000000007550, 2.560763078121147451 ) ) ;
#9074 = LINE ( 'NONE', #8921, #2544 ) ;
#9075 = CARTESIAN_POINT ( 'NONE',  ( -86.77438362643999881, 65.17411849586700612, -150.4984795835770228 ) ) ;
#9076 = CARTESIAN_POINT ( 'NONE',  ( 4.119136937081602667, 2.375954066961626143, 1.865445541641002514 ) ) ;
#9077 = CARTESIAN_POINT ( 'NONE',  ( -2.641694630006354405, -1.640624999999979572, 3.221290409975102520 ) ) ;
#9078 = DIRECTION ( 'NONE',  ( 0.000000000000000000, 0.000000000000000000, 1.000000000000000000 ) ) ;
#9079 = FACE_OUTER_BOUND ( 'NONE', #8915, .T. ) ;
#9080 = VECTOR ( 'NONE', #6067, 1000.000000000000000 ) ;
#9081 = ORIENTED_EDGE ( 'NONE', *, *, #2483, .F. ) ;
#9082 = DIRECTION ( 'NONE',  ( 0.000000000000000000, 0.000000000000000000, -1.000000000000000000 ) ) ;
#9083 = ORIENTED_EDGE ( 'NONE', *, *, #14092, .T. ) ;
#9084 = ORIENTED_EDGE ( 'NONE', *, *, #5854, .F. ) ;
#9085 = VERTEX_POINT ( 'NONE', #810 ) ;
#9086 = CARTESIAN_POINT ( 'NONE',  ( -69.77438362644001302, 82.17411849586700612, -183.7533135795160320 ) ) ;
#9087 = CIRCLE ( 'NONE', #10076, 3.499999999999999556 ) ;
#9088 = CARTESIAN_POINT ( 'NONE',  ( -2.211816241884709822, -3.944375000000018172, -2.696513105594267046 ) ) ;
#9089 = VECTOR ( 'NONE', #6413, 1000.000000000000000 ) ;
#9090 = CARTESIAN_POINT ( 'NONE',  ( 5.196152422706631135, 0.1227504548087541975, -1.122964458370237425E-15 ) ) ;
#9091 = CARTESIAN_POINT ( 'NONE',  ( -68.09912303623742957, 75.17411849586700612, -44.18949531478455128 ) ) ;
#9092 = CARTESIAN_POINT ( 'NONE',  ( -69.77438362644001302, 82.17411849586700612, -183.7533135795160320 ) ) ;
#9093 = DIRECTION ( 'NONE',  ( 0.000000000000000000, 1.000000000000000000, 0.000000000000000000 ) ) ;
#9094 = CARTESIAN_POINT ( 'NONE',  ( -0.9842438906765387241, -0.4995676945082616061, 3.993364550929547896 ) ) ;
#9095 = FACE_OUTER_BOUND ( 'NONE', #11776, .T. ) ;
#9096 = ORIENTED_EDGE ( 'NONE', *, *, #9503, .F. ) ;
#9097 = CARTESIAN_POINT ( 'NONE',  ( -69.77438362644001302, 82.17411849586700612, -138.4984795835769944 ) ) ;
#9098 = ORIENTED_EDGE ( 'NONE', *, *, #2600, .T. ) ;
#9099 = CIRCLE ( 'NONE', #10093, 2.042000000000002036 ) ;
#9100 = DIRECTION ( 'NONE',  ( 0.000000000000000000, 0.000000000000000000, 1.000000000000000000 ) ) ;
#9101 = VERTEX_POINT ( 'NONE', #7810 ) ;
#9102 = CARTESIAN_POINT ( 'NONE',  ( -3.490494984142799684, -1.406250000000081268, -2.330449509171077516 ) ) ;
#9103 = EDGE_LOOP ( 'NONE', ( #1122, #3805, #4056, #10218 ) ) ;
#9104 = CARTESIAN_POINT ( 'NONE',  ( -3.042761669814863623, -3.389838562372958997, -2.495273549889642783 ) ) ;
#9105 = DIRECTION ( 'NONE',  ( -1.000000000000000000, -1.682335022489801357E-15, 0.000000000000000000 ) ) ;
#9106 = ADVANCED_FACE ( 'NONE', ( #10268 ), #2057, .F. ) ;
#9107 = FACE_OUTER_BOUND ( 'NONE', #1316, .T. ) ;
#9108 = APPLICATION_CONTEXT ( 'automotive_design' ) ;
#9109 = AXIS2_PLACEMENT_3D ( 'NONE', #14267, #10619, #3483 ) ;
#9110 = CARTESIAN_POINT ( 'NONE',  ( -73.64736697264332577, 89.17411849586700612, -44.99847958359595168 ) ) ;
#9111 = ADVANCED_FACE ( 'NONE', ( #4391 ), #4066, .F. ) ;
#9112 = DIRECTION ( 'NONE',  ( 0.000000000000000000, -1.000000000000000000, 0.000000000000000000 ) ) ;
#9113 = FACE_OUTER_BOUND ( 'NONE', #8138, .T. ) ;
#9114 = DIRECTION ( 'NONE',  ( -0.1306536911286110270, 0.8634865235224290503, 0.4871556596095533709 ) ) ;
#9115 = ORIENTED_EDGE ( 'NONE', *, *, #3421, .T. ) ;
#9116 = CIRCLE ( 'NONE', #9109, 2.750000000000002665 ) ;
#9117 = CARTESIAN_POINT ( 'NONE',  ( -3.976927128516821952, -0.1006259897310525647, 0.3906606232675428059 ) ) ;
#9118 = ORIENTED_EDGE ( 'NONE', *, *, #13892, .T. ) ;
#9119 = CARTESIAN_POINT ( 'NONE',  ( 3.341236413112389947, -1.663124999999897824, -1.787503410618120459 ) ) ;
#9120 = CARTESIAN_POINT ( 'NONE',  ( -2.598076211353316012, 0.1227504548087343245, -4.499999999999999112 ) ) ;
#9121 = EDGE_CURVE ( 'NONE', #3945, #10174, #11523, .T. ) ;
#9122 = LINE ( 'NONE', #10127, #6160 ) ;
#9123 = CARTESIAN_POINT ( 'NONE',  ( -62.02799568714584666, 60.67411849586701322, -79.59847958357700293 ) ) ;
#9124 = AXIS2_PLACEMENT_3D ( 'NONE', #9653, #3541, #200 ) ;
#9125 = CARTESIAN_POINT ( 'NONE',  ( 3.980852709490799501, -0.4995676945082488940, -0.4039315514682934039 ) ) ;
#9126 =( LENGTH_UNIT ( ) NAMED_UNIT ( * ) SI_UNIT ( .MILLI., .METRE. ) );
#9127 = PLANE ( 'NONE',  #2116 ) ;
#9128 = CARTESIAN_POINT ( 'NONE',  ( -42.77438362644000591, 65.17411849586700612, -15.85886927678779834 ) ) ;
#9129 = ORIENTED_EDGE ( 'NONE', *, *, #13227, .F. ) ;
#9130 = CARTESIAN_POINT ( 'NONE',  ( -15.50000000000000000, 0.000000000000000000, 22.50000000000000000 ) ) ;
#9131 = ORIENTED_EDGE ( 'NONE', *, *, #7188, .F. ) ;
#9132 = ADVANCED_FACE ( 'NONE', ( #4462 ), #9179, .T. ) ;
#9133 = ORIENTED_EDGE ( 'NONE', *, *, #1265, .F. ) ;
#9134 = VERTEX_POINT ( 'NONE', #8258 ) ;
#9135 = ADVANCED_FACE ( 'NONE', ( #4699 ), #14308, .F. ) ;
#9136 = VERTEX_POINT ( 'NONE', #2206 ) ;
#9137 = ORIENTED_EDGE ( 'NONE', *, *, #4971, .F. ) ;
#9138 = CARTESIAN_POINT ( 'NONE',  ( -1.970263329862414148, -6.342963562372986530, -2.946344977785408936 ) ) ;
#9139 = CARTESIAN_POINT ( 'NONE',  ( -1.470831194960214861, -1.272500000000085230, 3.548278161707651090 ) ) ;
#9140 = EDGE_CURVE ( 'NONE', #15255, #7295, #4808, .T. ) ;
#9141 = DIRECTION ( 'NONE',  ( 1.000000000000000000, 2.551930889570660354E-15, 0.000000000000000000 ) ) ;
#9142 = CARTESIAN_POINT ( 'NONE',  ( 4.043635966909349122, -1.968749999999958034, 0.8028061105223156524 ) ) ;
#9143 = CARTESIAN_POINT ( 'NONE',  ( -52.77438362644000591, 99.17411849586700612, -145.4984795835769660 ) ) ;
#9144 = DIRECTION ( 'NONE',  ( 1.000000000000000000, 0.000000000000000000, 0.000000000000000000 ) ) ;
#9145 = ADVANCED_FACE ( 'NONE', ( #5792 ), #12235, .F. ) ;
#9146 = EDGE_CURVE ( 'NONE', #10133, #4759, #2360, .T. ) ;
#9147 = CARTESIAN_POINT ( 'NONE',  ( 5.196152422706626695, 1.678847577293385296, -1.115338501812287204E-15 ) ) ;
#9148 = CARTESIAN_POINT ( 'NONE',  ( -77.89938362643999881, 82.17411849586700612, -138.4984795835769944 ) ) ;
#9149 = CARTESIAN_POINT ( 'NONE',  ( -61.64938362644000591, 82.17411849586700612, -79.49847958357700861 ) ) ;
#9150 = CARTESIAN_POINT ( 'NONE',  ( -69.77438362644001302, 82.17411849586700612, -43.99847958357699440 ) ) ;
#9151 = EDGE_LOOP ( 'NONE', ( #13650, #9917, #2, #8096, #12569 ) ) ;
#9152 = B_SPLINE_CURVE_WITH_KNOTS ( 'NONE', 3,
 ( #8675, #7381, #5041, #9754, #14490, #13419 ),
 .UNSPECIFIED., .F., .F.,
 ( 4, 2, 4 ),
 ( 0.0002380763768132926339, 0.7291065797294586925, 1.457975083082104106 ),
 .UNSPECIFIED. ) ;
#9153 = DIRECTION ( 'NONE',  ( -1.000000000000000000, 0.000000000000000000, 0.000000000000000000 ) ) ;
#9154 = VERTEX_POINT ( 'NONE', #13088 ) ;
#9155 = EDGE_CURVE ( 'NONE', #9779, #7838, #1269, .T. ) ;
#9156 = VERTEX_POINT ( 'NONE', #2440 ) ;
#9157 = ORIENTED_EDGE ( 'NONE', *, *, #1992, .F. ) ;
#9158 = CARTESIAN_POINT ( 'NONE',  ( -101.2743836264399988, 111.1741184958670061, -67.49847958357700861 ) ) ;
#9159 = ADVANCED_FACE ( 'NONE', ( #7113 ), #5718, .T. ) ;
#9160 = DIRECTION ( 'NONE',  ( 2.551930889570660354E-15, -1.000000000000000000, 0.000000000000000000 ) ) ;
#9161 = CARTESIAN_POINT ( 'NONE',  ( 3.464101615137754386, 8.643436132524853256E-15, 2.999999999999999112 ) ) ;
#9162 = DIRECTION ( 'NONE',  ( -1.000000000000000000, -2.505711687522054122E-15, 0.000000000000000000 ) ) ;
#9163 = DIRECTION ( 'NONE',  ( 0.000000000000000000, 0.000000000000000000, -1.000000000000000000 ) ) ;
#9164 = DIRECTION ( 'NONE',  ( -9.422394424380278809E-16, 1.000000000000000000, -0.000000000000000000 ) ) ;
#9165 = CARTESIAN_POINT ( 'NONE',  ( -3.667454075173111505, -0.4995676945082688225, 2.138331822535261217 ) ) ;
#9166 = CARTESIAN_POINT ( 'NONE',  ( 22.58164641901421632, 11.99999970914576330, -11.73358795631400753 ) ) ;
#9167 = ORIENTED_EDGE ( 'NONE', *, *, #13109, .F. ) ;
#9168 = CARTESIAN_POINT ( 'NONE',  ( 23.42650720483347371, -1.718469852516944459E-15, 60.43630737906597261 ) ) ;
#9169 = ORIENTED_EDGE ( 'NONE', *, *, #5262, .F. ) ;
#9170 = VERTEX_POINT ( 'NONE', #105 ) ;
#9171 = ORIENTED_EDGE ( 'NONE', *, *, #421, .F. ) ;
#9172 = CARTESIAN_POINT ( 'NONE',  ( 3.757405615841324042, -0.9218749999999823475, 2.009662442622283773 ) ) ;
#9173 = ORIENTED_EDGE ( 'NONE', *, *, #11510, .F. ) ;
#9174 = CARTESIAN_POINT ( 'NONE',  ( -3.143458222507559352, -2.389838562372920805, -2.581159584719012745 ) ) ;
#9175 = CYLINDRICAL_SURFACE ( 'NONE', #11683, 4.500000000000003553 ) ;
#9176 = DIRECTION ( 'NONE',  ( 0.8660254037844485886, 0.000000000000000000, -0.4999999999999827360 ) ) ;
#9177 = VECTOR ( 'NONE', #8122, 1000.000000000000227 ) ;
#9178 = CARTESIAN_POINT ( 'NONE',  ( 22.58164641901421632, -12.00000029085423670, -14.13358795631400611 ) ) ;
#9179 = CYLINDRICAL_SURFACE ( 'NONE', #14212, 8.000000000000007105 ) ;
#9180 = CARTESIAN_POINT ( 'NONE',  ( 1.274862231047225439E-15, -0.4995676945082591081, 0.000000000000000000 ) ) ;
#9181 = CARTESIAN_POINT ( 'NONE',  ( 15.50000000000000000, -2.500000000000000000, 21.05662432702600029 ) ) ;
#9182 = AXIS2_PLACEMENT_3D ( 'NONE', #4855, #2511, #14148 ) ;
#9183 = DIRECTION ( 'NONE',  ( 1.000000000000000000, 0.000000000000000000, 0.000000000000000000 ) ) ;
#9184 = ORIENTED_EDGE ( 'NONE', *, *, #9593, .T. ) ;
#9185 = CIRCLE ( 'NONE', #4249, 3.000000000000002665 ) ;
#9186 = FILL_AREA_STYLE_COLOUR ( '', #11035 ) ;
#9187 = CARTESIAN_POINT ( 'NONE',  ( 1.843713500184434917, -0.7568749999999383471, -3.447171040406491027 ) ) ;
#9188 = EDGE_LOOP ( 'NONE', ( #10602, #8983, #13300, #1816, #8206 ) ) ;
#9189 = ADVANCED_FACE ( 'NONE', ( #11907 ), #3309, .T. ) ;
#9190 = CARTESIAN_POINT ( 'NONE',  ( 3.515159614179530045, -2.538124999999942677, 1.067305873498098912 ) ) ;
#9191 = LINE ( 'NONE', #3010, #1516 ) ;
#9192 = VECTOR ( 'NONE', #2355, 1000.000000000000000 ) ;
#9193 = CARTESIAN_POINT ( 'NONE',  ( -1.673688575075004152E-15, 4.650702586819541295, 0.000000000000000000 ) ) ;
#9194 = CARTESIAN_POINT ( 'NONE',  ( 66.41329019055578442, 0.000000000000000000, 137.5095611191910621 ) ) ;
#9195 = DIRECTION ( 'NONE',  ( 0.000000000000000000, 0.000000000000000000, -1.000000000000000000 ) ) ;
#9196 = AXIS2_PLACEMENT_3D ( 'NONE', #9280, #10518, #13021 ) ;
#9197 = FACE_OUTER_BOUND ( 'NONE', #10321, .T. ) ;
#9198 = ORIENTED_EDGE ( 'NONE', *, *, #4941, .T. ) ;
#9199 = CARTESIAN_POINT ( 'NONE',  ( -85.77438362644001302, 82.17411849586700612, -183.7533135795160320 ) ) ;
#9200 = EDGE_CURVE ( 'NONE', #856, #11342, #15307, .T. ) ;
#9201 = VERTEX_POINT ( 'NONE', #14001 ) ;
#9202 = TOROIDAL_SURFACE ( 'NONE', #11695, 2.931404194366992400, 0.5000000000000000000 ) ;
#9203 = ORIENTED_EDGE ( 'NONE', *, *, #4227, .T. ) ;
#9204 = CARTESIAN_POINT ( 'NONE',  ( 3.384491019838402170, -4.600625000000129639, -0.3324735777645302370 ) ) ;
#9205 = VERTEX_POINT ( 'NONE', #6034 ) ;
#9206 = VERTEX_POINT ( 'NONE', #8415 ) ;
#9207 = B_SPLINE_CURVE_WITH_KNOTS ( 'NONE', 3,
 ( #664, #5417, #12544, #4238 ),
 .UNSPECIFIED., .F., .F.,
 ( 4, 4 ),
 ( 2.309401076754191683E-07, 0.002598307151460994141 ),
 .UNSPECIFIED. ) ;
#9208 = ADVANCED_FACE ( 'NONE', ( #3449 ), #10739, .T. ) ;
#9209 = ORIENTED_EDGE ( 'NONE', *, *, #14456, .T. ) ;
#9210 = DIRECTION ( 'NONE',  ( 0.000000000000000000, 1.000000000000000000, 0.000000000000000000 ) ) ;
#9211 = VECTOR ( 'NONE', #2443, 1000.000000000000000 ) ;
#9212 = CARTESIAN_POINT ( 'NONE',  ( -0.3809421545647762031, -0.8506249999999871969, -3.878187885777538035 ) ) ;
#9213 = DIRECTION ( 'NONE',  ( 0.000000000000000000, 1.000000000000000000, 0.000000000000000000 ) ) ;
#9214 = CARTESIAN_POINT ( 'NONE',  ( 0.8105829119240891556, -1.781250000000002887, 4.067378511145360420 ) ) ;
#9215 = CARTESIAN_POINT ( 'NONE',  ( -62.02799568714584666, 59.67411849586701322, -152.4984795835769944 ) ) ;
#9216 = CARTESIAN_POINT ( 'NONE',  ( -104.2743836264399988, 72.17411849586700612, -67.49847958357700861 ) ) ;
#9217 = PRESENTATION_LAYER_ASSIGNMENT (  '', '', ( #11956 ) ) ;
#9218 = DIRECTION ( 'NONE',  ( 0.000000000000000000, 0.000000000000000000, -1.000000000000000000 ) ) ;
#9219 = CARTESIAN_POINT ( 'NONE',  ( 1.951563910473907981E-15, 7.362500000000000711, 0.000000000000000000 ) ) ;
#9220 = PLANE ( 'NONE',  #11773 ) ;
#9221 = DIRECTION ( 'NONE',  ( 1.000000000000000000, 0.000000000000000000, -0.000000000000000000 ) ) ;
#9222 = CARTESIAN_POINT ( 'NONE',  ( -61.64938362644000591, 82.17411849586700612, -138.4984795835769944 ) ) ;
#9223 = ORIENTED_EDGE ( 'NONE', *, *, #194, .F. ) ;
#9224 = LINE ( 'NONE', #12729, #8746 ) ;
#9225 = AXIS2_PLACEMENT_3D ( 'NONE', #6914, #1073, #8144 ) ;
#9226 = ADVANCED_FACE ( 'NONE', ( #13157 ), #8765, .F. ) ;
#9227 = ORIENTED_EDGE ( 'NONE', *, *, #1373, .F. ) ;
#9228 = VERTEX_POINT ( 'NONE', #5959 ) ;
#9229 = VERTEX_POINT ( 'NONE', #12844 ) ;
#9230 = ADVANCED_FACE ( 'NONE', ( #14228 ), #3609, .F. ) ;
#9231 = AXIS2_PLACEMENT_3D ( 'NONE', #6580, #4085, #2997 ) ;
#9232 = DIRECTION ( 'NONE',  ( 0.9961946980917453232, -7.200509705930740925E-17, 0.08715574274766159368 ) ) ;
#9233 = ADVANCED_FACE ( 'NONE', ( #4538 ), #3376, .T. ) ;
#9234 = CARTESIAN_POINT ( 'NONE',  ( -2.465526969817838587, -3.960000000000052811, -2.463696919996925416 ) ) ;
#9235 = DIRECTION ( 'NONE',  ( -0.9961946980917453232, 7.200509705930739692E-17, -0.08715574274766156593 ) ) ;
#9236 = FACE_OUTER_BOUND ( 'NONE', #13583, .T. ) ;
#9237 = CARTESIAN_POINT ( 'NONE',  ( -13.41835358098578723, 11.99999970914575975, -8.183940086454237317 ) ) ;
#9238 = AXIS2_PLACEMENT_3D ( 'NONE', #12359, #10017, #12428 ) ;
#9239 = DIRECTION ( 'NONE',  ( 0.000000000000000000, -1.000000000000000000, 0.000000000000000000 ) ) ;
#9240 = EDGE_CURVE ( 'NONE', #11859, #12075, #6977, .T. ) ;
#9241 = FACE_OUTER_BOUND ( 'NONE', #3415, .T. ) ;
#9242 = CARTESIAN_POINT ( 'NONE',  ( 15.50000000000000000, -1.037157890325000054, -22.50000000000000000 ) ) ;
#9243 = CIRCLE ( 'NONE', #11234, 1.999999999999986233 ) ;
#9244 = EDGE_LOOP ( 'NONE', ( #6455, #12622 ) ) ;
#9245 = CARTESIAN_POINT ( 'NONE',  ( 37.35543536254874653, -3.618985300545107364, 6.000000000000000000 ) ) ;
#9246 = ADVANCED_FACE ( 'NONE', ( #2826 ), #14385, .T. ) ;
#9247 = VERTEX_POINT ( 'NONE', #1667 ) ;
#9248 = DIRECTION ( 'NONE',  ( 0.000000000000000000, 0.000000000000000000, -1.000000000000000000 ) ) ;
#9249 = CIRCLE ( 'NONE', #5309, 3.749999999999996447 ) ;
#9250 = EDGE_LOOP ( 'NONE', ( #10137, #13145, #13966, #6377 ) ) ;
#9251 = CIRCLE ( 'NONE', #3815, 3.750000000000003553 ) ;
#9252 = EDGE_CURVE ( 'NONE', #11928, #4340, #12140, .T. ) ;
#9253 = CARTESIAN_POINT ( 'NONE',  ( 4.232448940998905229, -0.9843749999998714362, 0.4153177470904050317 ) ) ;
#9254 = ADVANCED_FACE ( 'NONE', ( #13464 ), #3985, .F. ) ;
#9255 = ORIENTED_EDGE ( 'NONE', *, *, #10758, .F. ) ;
#9256 = CARTESIAN_POINT ( 'NONE',  ( -2.558190236227187331, -2.639838562373072239, 3.119474918453590373 ) ) ;
#9257 =( BOUNDED_CURVE ( )  B_SPLINE_CURVE ( 3, ( #5851, #13134, #7004, #8318 ),
 .UNSPECIFIED., .F., .T. ) 
 B_SPLINE_CURVE_WITH_KNOTS ( ( 4, 4 ),
 ( 1.570796326794896780, 3.141592653589793116 ),
 .UNSPECIFIED. ) 
 CURVE ( )  GEOMETRIC_REPRESENTATION_ITEM ( )  RATIONAL_B_SPLINE_CURVE ( ( 1.000000000000000000, 0.8047378541243650485, 0.8047378541243650485, 1.000000000000000000 ) ) 
 REPRESENTATION_ITEM ( '' )  );
#9258 = CARTESIAN_POINT ( 'NONE',  ( -38.27438362644000591, 57.67411849586700612, -67.49847958357700861 ) ) ;
#9259 = PLANE ( 'NONE',  #11050 ) ;
#9260 = CARTESIAN_POINT ( 'NONE',  ( 3.012508034349780761, 2.058119353682402952, -3.782183026296719763 ) ) ;
#9261 = AXIS2_PLACEMENT_3D ( 'NONE', #4655, #8291, #5827 ) ;
#9262 = AXIS2_PLACEMENT_3D ( 'NONE', #6373, #7297, #10779 ) ;
#9263 = DIRECTION ( 'NONE',  ( 1.000000000000000000, 0.000000000000000000, 0.000000000000000000 ) ) ;
#9264 = ORIENTED_EDGE ( 'NONE', *, *, #7879, .T. ) ;
#9265 = CARTESIAN_POINT ( 'NONE',  ( 3.155399193331007712, -5.123732279192288352, -1.903239753125236078 ) ) ;
#9266 = DIRECTION ( 'NONE',  ( -0.4999999999999998890, 0.000000000000000000, 0.8660254037844387076 ) ) ;
#9267 = EDGE_LOOP ( 'NONE', ( #4344, #3637, #6402, #14002, #12336 ) ) ;
#9268 = DIRECTION ( 'NONE',  ( 0.8660254037844387076, 0.4999999999999998890, 0.000000000000000000 ) ) ;
#9269 = CARTESIAN_POINT ( 'NONE',  ( 3.555702576009056148, -5.046874999999973355, -1.077603027457875395 ) ) ;
#9270 = ORIENTED_EDGE ( 'NONE', *, *, #14893, .T. ) ;
#9271 = CLOSED_SHELL ( 'NONE', ( #6200, #6952, #1761, #5264, #11908, #11232, #13346, #10267, #12652, #12492, #13942, #2602 ) ) ;
#9272 = VECTOR ( 'NONE', #3589, 1000.000000000000114 ) ;
#9273 = CARTESIAN_POINT ( 'NONE',  ( 3.039561480324906029, -2.678749999999966214, -2.029833227700108544 ) ) ;
#9274 = DIRECTION ( 'NONE',  ( 0.000000000000000000, 0.000000000000000000, -1.000000000000000000 ) ) ;
#9275 = CARTESIAN_POINT ( 'NONE',  ( -69.77438362644001302, 90.17411849586700612, -79.59847958357700293 ) ) ;
#9276 = DIRECTION ( 'NONE',  ( -1.000000000000000000, 0.000000000000000000, -0.000000000000000000 ) ) ;
#9277 = DIRECTION ( 'NONE',  ( 0.000000000000000000, 0.000000000000000000, -1.000000000000000000 ) ) ;
#9278 = SURFACE_STYLE_USAGE ( .BOTH. , #978 ) ;
#9279 = CARTESIAN_POINT ( 'NONE',  ( -69.77438362644001302, 94.57411849586699759, -89.99847958357699440 ) ) ;
#9280 = CARTESIAN_POINT ( 'NONE',  ( -86.77438362644001302, 57.67411849586700612, -15.85886927678779834 ) ) ;
#9281 = AXIS2_PLACEMENT_3D ( 'NONE', #11879, #1244, #4591 ) ;
#9282 = ORIENTED_EDGE ( 'NONE', *, *, #1640, .T. ) ;
#9283 = B_SPLINE_CURVE_WITH_KNOTS ( 'NONE', 3,
 ( #6743, #8980, #11464, #4408 ),
 .UNSPECIFIED., .F., .F.,
 ( 4, 4 ),
 ( 0.000000000000000000, 0.0004097632218424854624 ),
 .UNSPECIFIED. ) ;
#9284 = CIRCLE ( 'NONE', #13512, 1.785937500000001066 ) ;
#9285 = CARTESIAN_POINT ( 'NONE',  ( -91.27438362643999881, 99.17411849586700612, -79.59847958357700293 ) ) ;
#9286 = VERTEX_POINT ( 'NONE', #8566 ) ;
#9287 = ORIENTED_EDGE ( 'NONE', *, *, #5767, .T. ) ;
#9288 = CARTESIAN_POINT ( 'NONE',  ( 2.417253850353039191, -4.460000000000003517, 2.418486108946755753 ) ) ;
#9289 = ORIENTED_EDGE ( 'NONE', *, *, #12013, .T. ) ;
#9290 = ORIENTED_EDGE ( 'NONE', *, *, #10959, .T. ) ;
#9291 = EDGE_LOOP ( 'NONE', ( #6347, #9325, #6057, #10791 ) ) ;
#9292 = CARTESIAN_POINT ( 'NONE',  ( 3.706442405453559630, -4.983588562372924358, 0.3636771760149511423 ) ) ;
#9293 = PRESENTATION_LAYER_ASSIGNMENT (  '', '', ( #126 ) ) ;
#9294 = AXIS2_PLACEMENT_3D ( 'NONE', #8607, #6156, #13191 ) ;
#9295 = DIRECTION ( 'NONE',  ( -1.000000000000000000, 0.000000000000000000, 0.000000000000000000 ) ) ;
#9296 = DIRECTION ( 'NONE',  ( -0.000000000000000000, -0.000000000000000000, -1.000000000000000000 ) ) ;
#9297 = EDGE_CURVE ( 'NONE', #686, #9229, #3989, .T. ) ;
#9298 = CARTESIAN_POINT ( 'NONE',  ( -4.130341191321600824, 2.356280171323974937, 1.846039204036427961 ) ) ;
#9299 = CARTESIAN_POINT ( 'NONE',  ( 4.781720599710156172, 2.058119353682408725, 0.7178169737032801256 ) ) ;
#9300 = CARTESIAN_POINT ( 'NONE',  ( -15.50000000000000000, -0.2038245569916614930, 21.05662432702600029 ) ) ;
#9301 = LINE ( 'NONE', #1000, #14236 ) ;
#9302 = DIRECTION ( 'NONE',  ( -1.000000000000000000, 0.000000000000000000, 0.000000000000000000 ) ) ;
#9303 = ADVANCED_FACE ( 'NONE', ( #5086 ), #13387, .F. ) ;
#9304 = CARTESIAN_POINT ( 'NONE',  ( 0.6569748927284305706, -4.803749999999888054, -3.309289439050846937 ) ) ;
#9305 = DIRECTION ( 'NONE',  ( 0.000000000000000000, 0.000000000000000000, -1.000000000000000000 ) ) ;
#9306 = VERTEX_POINT ( 'NONE', #14531 ) ;
#9307 = DIRECTION ( 'NONE',  ( 0.000000000000000000, 0.000000000000000000, 1.000000000000000000 ) ) ;
#9308 = ORIENTED_EDGE ( 'NONE', *, *, #4605, .T. ) ;
#9309 = VECTOR ( 'NONE', #10897, 1000.000000000000000 ) ;
#9310 = ORIENTED_EDGE ( 'NONE', *, *, #5174, .F. ) ;
#9311 = VERTEX_POINT ( 'NONE', #8796 ) ;
#9312 = VECTOR ( 'NONE', #7360, 1000.000000000000114 ) ;
#9313 = APPLICATION_CONTEXT ( 'automotive_design' ) ;
#9314 = CIRCLE ( 'NONE', #3379, 4.296275033669348709 ) ;
#9315 = DIRECTION ( 'NONE',  ( 1.000000000000000000, 0.000000000000000000, 0.000000000000000000 ) ) ;
#9316 = CARTESIAN_POINT ( 'NONE',  ( -75.64713719066081410, 66.22072495173567575, -81.84847958357697451 ) ) ;
#9317 = ADVANCED_FACE ( 'NONE', ( #7339 ), #13313, .T. ) ;
#9318 = FACE_OUTER_BOUND ( 'NONE', #4153, .T. ) ;
#9319 = AXIS2_PLACEMENT_3D ( 'NONE', #6781, #11352, #717 ) ;
#9320 = DIRECTION ( 'NONE',  ( 0.9375000000000004441, 0.000000000000000000, 0.3479852726768752902 ) ) ;
#9321 = PLANE ( 'NONE',  #6792 ) ;
#9322 = AXIS2_PLACEMENT_3D ( 'NONE', #10395, #10944, #9923 ) ;
#9323 = CARTESIAN_POINT ( 'NONE',  ( -13.41835358098578723, 11.99999970914576330, -11.73358795631400397 ) ) ;
#9324 = DIRECTION ( 'NONE',  ( -2.551930889570659960E-15, 1.000000000000000000, 0.000000000000000000 ) ) ;
#9325 = ORIENTED_EDGE ( 'NONE', *, *, #4599, .F. ) ;
#9326 = DIRECTION ( 'NONE',  ( -0.8660254037844482555, 0.000000000000000000, 0.4999999999999831801 ) ) ;
#9327 = ORIENTED_EDGE ( 'NONE', *, *, #10190, .F. ) ;
#9328 = EDGE_LOOP ( 'NONE', ( #10628, #4723, #6773, #2153 ) ) ;
#9329 = CARTESIAN_POINT ( 'NONE',  ( -89.27438362644100778, 110.1741184958670061, -79.59847958357700293 ) ) ;
#9330 = AXIS2_PLACEMENT_3D ( 'NONE', #3687, #10741, #9801 ) ;
#9331 = EDGE_LOOP ( 'NONE', ( #7746, #12342, #9223 ) ) ;
#9332 = EDGE_CURVE ( 'NONE', #7325, #12075, #8940, .T. ) ;
#9333 = CARTESIAN_POINT ( 'NONE',  ( -3.873284713637146215, -1.437499999999919620, -1.605572741981209139 ) ) ;
#9334 = ORIENTED_EDGE ( 'NONE', *, *, #14709, .F. ) ;
#9335 = EDGE_CURVE ( 'NONE', #13360, #8700, #1764, .T. ) ;
#9336 = CARTESIAN_POINT ( 'NONE',  ( -3.358725955652476891, -2.592963562373010955, 2.245994589438188971 ) ) ;
#9337 = CARTESIAN_POINT ( 'NONE',  ( -42.77438362644000591, 110.1741184958670061, -152.4984795835769944 ) ) ;
#9338 = EDGE_CURVE ( 'NONE', #1550, #6249, #6114, .T. ) ;
#9339 = FACE_BOUND ( 'NONE', #687, .T. ) ;
#9340 = FACE_OUTER_BOUND ( 'NONE', #13051, .T. ) ;
#9341 = ADVANCED_FACE ( 'NONE', ( #187 ), #2674, .F. ) ;
#9342 = AXIS2_PLACEMENT_3D ( 'NONE', #10927, #1539, #6514 ) ;
#9343 = DIRECTION ( 'NONE',  ( 0.000000000000000000, 1.000000000000000000, 0.000000000000000000 ) ) ;
#9344 = EDGE_CURVE ( 'NONE', #4564, #10086, #1017, .T. ) ;
#9345 = ORIENTED_EDGE ( 'NONE', *, *, #8769, .F. ) ;
#9346 = CARTESIAN_POINT ( 'NONE',  ( -52.77438362644100067, 101.5320169952374414, -147.9984795835769944 ) ) ;
#9347 = ORIENTED_EDGE ( 'NONE', *, *, #769, .T. ) ;
#9348 =( BOUNDED_CURVE ( )  B_SPLINE_CURVE ( 3, ( #6519, #8979, #7683, #6674 ),
 .UNSPECIFIED., .F., .T. ) 
 B_SPLINE_CURVE_WITH_KNOTS ( ( 4, 4 ),
 ( 3.141592653589793116, 4.712388980384689674 ),
 .UNSPECIFIED. ) 
 CURVE ( )  GEOMETRIC_REPRESENTATION_ITEM ( )  RATIONAL_B_SPLINE_CURVE ( ( 1.000000000000000000, 0.8047378541243649375, 0.8047378541243649375, 1.000000000000000000 ) ) 
 REPRESENTATION_ITEM ( '' )  );
#9349 = CARTESIAN_POINT ( 'NONE',  ( -14.45313394609757651, -0.2715358723599896051, 21.66103272505202781 ) ) ;
#9350 = CARTESIAN_POINT ( 'NONE',  ( -3.589096097608166058, -5.468749999999688249, -0.7148808183696577778 ) ) ;
#9351 = ORIENTED_EDGE ( 'NONE', *, *, #13188, .T. ) ;
#9352 = CIRCLE ( 'NONE', #4660, 4.249999999999996447 ) ;
#9353 = CARTESIAN_POINT ( 'NONE',  ( 2.315514200798038047, -2.725624999999891607, -2.819975302942780537 ) ) ;
#9354 = EDGE_CURVE ( 'NONE', #3787, #6469, #10926, .T. ) ;
#9355 = DIRECTION ( 'NONE',  ( -1.000000000000000000, 0.000000000000000000, 0.000000000000000000 ) ) ;
#9356 = DIRECTION ( 'NONE',  ( 1.000000000000000000, 0.000000000000000000, 0.000000000000000000 ) ) ;
#9357 = FACE_OUTER_BOUND ( 'NONE', #14366, .T. ) ;
#9358 = FACE_OUTER_BOUND ( 'NONE', #2119, .T. ) ;
#9359 = DIRECTION ( 'NONE',  ( 0.000000000000000000, 0.000000000000000000, 1.000000000000000000 ) ) ;
#9360 = DIRECTION ( 'NONE',  ( 0.000000000000000000, 0.000000000000000000, -1.000000000000000000 ) ) ;
#9361 = CIRCLE ( 'NONE', #14079, 4.500000000000003553 ) ;
#9362 = ORIENTED_EDGE ( 'NONE', *, *, #11325, .T. ) ;
#9363 = DIRECTION ( 'NONE',  ( -1.000000000000000000, 0.000000000000000000, 0.000000000000000000 ) ) ;
#9364 = ORIENTED_EDGE ( 'NONE', *, *, #2329, .F. ) ;
#9365 = ORIENTED_EDGE ( 'NONE', *, *, #10822, .F. ) ;
#9366 = CARTESIAN_POINT ( 'NONE',  ( -2.189584623831577037, -4.225624999999936016, 2.666627758504862111 ) ) ;
#9367 = ORIENTED_EDGE ( 'NONE', *, *, #2989, .F. ) ;
#9368 = VERTEX_POINT ( 'NONE', #6191 ) ;
#9369 = VERTEX_POINT ( 'NONE', #9643 ) ;
#9370 = CARTESIAN_POINT ( 'NONE',  ( -2.414341998011519497, -4.358588562372940345, -2.943449326273882338 ) ) ;
#9371 = DIRECTION ( 'NONE',  ( 0.000000000000000000, -1.000000000000000000, 0.000000000000000000 ) ) ;
#9372 = AXIS2_PLACEMENT_3D ( 'NONE', #5271, #14637, #9985 ) ;
#9373 = FACE_OUTER_BOUND ( 'NONE', #4539, .T. ) ;
#9374 = DIRECTION ( 'NONE',  ( 1.000000000000000000, 0.000000000000000000, 0.000000000000000000 ) ) ;
#9375 = PLANE ( 'NONE',  #7861 ) ;
#9376 = CARTESIAN_POINT ( 'NONE',  ( 22.46142565487374299, 5.000000000000000000, 22.46142565487405918 ) ) ;
#9377 = CARTESIAN_POINT ( 'NONE',  ( -86.77438362644100778, 99.17411849586700612, -147.9984795835769944 ) ) ;
#9378 = CARTESIAN_POINT ( 'NONE',  ( -15.50000000000000000, -0.4000000000005236034, 25.79999999999947136 ) ) ;
#9379 = CARTESIAN_POINT ( 'NONE',  ( -84.73238362644100619, 97.99516924618178848, -150.4984795835770228 ) ) ;
#9380 = CARTESIAN_POINT ( 'NONE',  ( 0.6449049195797605938, -5.366250000000259313, 3.235821967343390337 ) ) ;
#9381 = CARTESIAN_POINT ( 'NONE',  ( -16.75000000000000000, -2.500000000000000000, -21.77831216351300014 ) ) ;
#9382 = VERTEX_POINT ( 'NONE', #5167 ) ;
#9383 = DIRECTION ( 'NONE',  ( 0.000000000000000000, 1.734723475976805517E-15, -1.000000000000000000 ) ) ;
#9384 = ORIENTED_EDGE ( 'NONE', *, *, #22, .T. ) ;
#9385 = ORIENTED_EDGE ( 'NONE', *, *, #12379, .T. ) ;
#9386 = VERTEX_POINT ( 'NONE', #10899 ) ;
#9387 = CARTESIAN_POINT ( 'NONE',  ( -83.02438362643998460, 65.17411849586700612, -150.4984795835770228 ) ) ;
#9388 = CARTESIAN_POINT ( 'NONE',  ( -0.3421672931279376995, -3.850625000000083009, -3.483230393025887661 ) ) ;
#9389 = ADVANCED_FACE ( 'NONE', ( #5004 ), #2503, .F. ) ;
#9390 = CARTESIAN_POINT ( 'NONE',  ( 15.50000000000000000, -0.4000000000005274892, 25.79999999999946780 ) ) ;
#9391 = CARTESIAN_POINT ( 'NONE',  ( 16.75000000000000000, -2.500000000000000000, -23.22168783648699986 ) ) ;
#9392 = CARTESIAN_POINT ( 'NONE',  ( -2.193587568844167279, 1.881091898548003183, -4.499999999999998224 ) ) ;
#9393 = CARTESIAN_POINT ( 'NONE',  ( -14.25000000000000000, -2.500000000000000000, -21.77831216351300014 ) ) ;
#9394 = DIRECTION ( 'NONE',  ( 0.000000000000000000, 0.000000000000000000, 1.000000000000000000 ) ) ;
#9395 = FACE_OUTER_BOUND ( 'NONE', #15316, .T. ) ;
#9396 = DIRECTION ( 'NONE',  ( 0.000000000000000000, 0.000000000000000000, 1.000000000000000000 ) ) ;
#9397 = CARTESIAN_POINT ( 'NONE',  ( 15.50000000000000000, -0.4000000000000000222, -25.99999999999999645 ) ) ;
#9398 = VERTEX_POINT ( 'NONE', #14455 ) ;
#9399 = CYLINDRICAL_SURFACE ( 'NONE', #179, 2.500000000000002220 ) ;
#9400 = ORIENTED_EDGE ( 'NONE', *, *, #10725, .F. ) ;
#9401 = ORIENTED_EDGE ( 'NONE', *, *, #11063, .T. ) ;
#9402 = EDGE_CURVE ( 'NONE', #12871, #12429, #5999, .T. ) ;
#9403 = CARTESIAN_POINT ( 'NONE',  ( 2.056459069434533049, -0.1718749999999378830, -3.844889943890866579 ) ) ;
#9404 = ORIENTED_EDGE ( 'NONE', *, *, #9802, .F. ) ;
#9405 = CARTESIAN_POINT ( 'NONE',  ( -2.854913087873755195, -2.624213562373173048, 2.853407187448114612 ) ) ;
#9406 = CARTESIAN_POINT ( 'NONE',  ( -86.77438362644100778, 96.81621999649657084, -147.9984795835769944 ) ) ;
#9407 = PLANE ( 'NONE',  #5366 ) ;
#9408 = CARTESIAN_POINT ( 'NONE',  ( 14.25000000000000178, -0.2714405302574884327, 22.98746066354537732 ) ) ;
#9409 = ADVANCED_FACE ( 'NONE', ( #8944 ), #15191, .F. ) ;
#9410 = CARTESIAN_POINT ( 'NONE',  ( 21.98164641901421135, -12.00000029085423670, -11.73358795631400930 ) ) ;
#9411 = ORIENTED_EDGE ( 'NONE', *, *, #14252, .T. ) ;
#9412 = DIRECTION ( 'NONE',  ( -1.000000000000000000, 0.000000000000000000, 0.000000000000000000 ) ) ;
#9413 = DIRECTION ( 'NONE',  ( 1.000000000000000000, 0.000000000000000000, 0.000000000000000000 ) ) ;
#9414 = ADVANCED_FACE ( 'NONE', ( #7794 ), #10104, .T. ) ;
#9415 = EDGE_LOOP ( 'NONE', ( #14247, #10139, #9062, #9334 ) ) ;
#9416 = PRESENTATION_STYLE_ASSIGNMENT (( #4705 ) ) ;
#9417 = CARTESIAN_POINT ( 'NONE',  ( 3.407468303614469285, -3.921874999999769074, 1.822475935421856708 ) ) ;
#9418 = ORIENTED_EDGE ( 'NONE', *, *, #6346, .F. ) ;
#9419 = ADVANCED_FACE ( 'NONE', ( #4220 ), #3750, .T. ) ;
#9420 = EDGE_CURVE ( 'NONE', #4633, #5514, #4998, .T. ) ;
#9421 = CARTESIAN_POINT ( 'NONE',  ( -3.456628223078394679, -2.022499999999918252, -1.432834870345867984 ) ) ;
#9422 = LINE ( 'NONE', #15159, #1427 ) ;
#9423 = CARTESIAN_POINT ( 'NONE',  ( -102.2743836264399988, 104.6741184958670061, -152.4984795835769944 ) ) ;
#9424 = AXIS2_PLACEMENT_3D ( 'NONE', #3914, #3758, #2909 ) ;
#9425 = EDGE_CURVE ( 'NONE', #1386, #4034, #12875, .T. ) ;
#9426 = CARTESIAN_POINT ( 'NONE',  ( -77.94906324475290660, 70.01464610989972925, -83.44847958357698303 ) ) ;
#9427 =( NAMED_UNIT ( * ) PLANE_ANGLE_UNIT ( ) SI_UNIT ( $, .RADIAN. ) );
#9428 = DIRECTION ( 'NONE',  ( -2.551930889570658776E-15, 1.000000000000000000, 0.000000000000000000 ) ) ;
#9429 = CARTESIAN_POINT ( 'NONE',  ( 15.50000000000000000, -0.4000000000000000222, -22.50000000000000000 ) ) ;
#9430 = AXIS2_PLACEMENT_3D ( 'NONE', #4246, #4327, #11457 ) ;
#9431 = ORIENTED_EDGE ( 'NONE', *, *, #3225, .F. ) ;
#9432 = DIRECTION ( 'NONE',  ( 0.000000000000000000, -0.9860132971832696880, 0.1666666666666656860 ) ) ;
#9433 = ADVANCED_FACE ( 'NONE', ( #9812 ), #11843, .T. ) ;
#9434 = EDGE_LOOP ( 'NONE', ( #10391, #7500, #10706, #14650, #15331 ) ) ;
#9435 = PRODUCT ( 'Part2', 'Part2', '', ( #7267 ) ) ;
#9436 = DIRECTION ( 'NONE',  ( 0.08715574274766123286, 0.000000000000000000, -0.9961946980917453232 ) ) ;
#9437 = CARTESIAN_POINT ( 'NONE',  ( -1.647113530155737360, -3.913124999999971099, -3.078783428963379531 ) ) ;
#9438 = ORIENTED_EDGE ( 'NONE', *, *, #10132, .T. ) ;
#9439 = ORIENTED_EDGE ( 'NONE', *, *, #11900, .F. ) ;
#9440 = ORIENTED_EDGE ( 'NONE', *, *, #4785, .F. ) ;
#9441 = CARTESIAN_POINT ( 'NONE',  ( 3.215963366055881512, -3.905463562372929243, 2.147137851111217799 ) ) ;
#9442 = CARTESIAN_POINT ( 'NONE',  ( -54.81638362644000040, 63.99516924618178848, -150.4984795835770228 ) ) ;
#9443 = VECTOR ( 'NONE', #9868, 1000.000000000000000 ) ;
#9444 = FACE_OUTER_BOUND ( 'NONE', #9415, .T. ) ;
#9445 = CIRCLE ( 'NONE', #4757, 4.362044368365340041 ) ;
#9446 = DIRECTION ( 'NONE',  ( -0.9961946980917452121, 7.200509705930738460E-17, -0.08715574274766156593 ) ) ;
#9447 = CARTESIAN_POINT ( 'NONE',  ( -9.503456061879928640, -12.00000029085427222, 69.60114695342350899 ) ) ;
#9448 = FACE_OUTER_BOUND ( 'NONE', #2065, .T. ) ;
#9449 = CARTESIAN_POINT ( 'NONE',  ( 26.96929424362929950, -1.434287255462209759E-15, 19.94206622808625440 ) ) ;
#9450 = CARTESIAN_POINT ( 'NONE',  ( -2.465526969817838587, -3.960000000000052811, -2.463696919996925416 ) ) ;
#9451 = DIRECTION ( 'NONE',  ( 0.000000000000000000, 0.000000000000000000, 1.000000000000000000 ) ) ;
#9452 = AXIS2_PLACEMENT_3D ( 'NONE', #8540, #12042, #14353 ) ;
#9453 = ORIENTED_EDGE ( 'NONE', *, *, #7925, .T. ) ;
#9454 = CARTESIAN_POINT ( 'NONE',  ( -1.629699455448989389E-14, 8.699999999999999289, 5.655858585055787181E-29 ) ) ;
#9455 = ORIENTED_EDGE ( 'NONE', *, *, #5726, .F. ) ;
#9456 = AXIS2_PLACEMENT_3D ( 'NONE', #9086, #2180, #7926 ) ;
#9457 = ORIENTED_EDGE ( 'NONE', *, *, #14536, .T. ) ;
#9458 = EDGE_LOOP ( 'NONE', ( #5799, #4259, #10319, #8762, #323 ) ) ;
#9459 = VECTOR ( 'NONE', #1015, 1000.000000000000000 ) ;
#9460 = DIRECTION ( 'NONE',  ( -1.000000000000000000, 0.000000000000000000, 0.000000000000000000 ) ) ;
#9461 = CARTESIAN_POINT ( 'NONE',  ( -3.335258087793214088, -3.022499999999893827, -1.380066378191329379 ) ) ;
#9462 = CARTESIAN_POINT ( 'NONE',  ( -52.77438362644100067, 96.81621999649657084, -147.9984795835769944 ) ) ;
#9463 = CARTESIAN_POINT ( 'NONE',  ( -15.50000000000000000, -0.1999999999999999556, 23.94999999999999929 ) ) ;
#9464 = CARTESIAN_POINT ( 'NONE',  ( -2.598076211353319565, 1.678847577293365978, -4.499999999999999112 ) ) ;
#9465 = PLANE ( 'NONE',  #14031 ) ;
#9466 = DIRECTION ( 'NONE',  ( -1.000000000000000000, 0.000000000000000000, 0.000000000000000000 ) ) ;
#9467 = DIRECTION ( 'NONE',  ( 0.000000000000000000, 0.000000000000000000, 1.000000000000000000 ) ) ;
#9468 = CARTESIAN_POINT ( 'NONE',  ( 57.41329019055577021, 2.488961461112888074, 99.29549861919106490 ) ) ;
#9469 = AXIS2_PLACEMENT_3D ( 'NONE', #509, #6430, #9816 ) ;
#9470 = DIRECTION ( 'NONE',  ( 0.000000000000000000, 0.000000000000000000, -1.000000000000000000 ) ) ;
#9471 = DIRECTION ( 'NONE',  ( 1.000000000000000000, 0.000000000000000000, 0.000000000000000000 ) ) ;
#9472 = VERTEX_POINT ( 'NONE', #7274 ) ;
#9473 = CARTESIAN_POINT ( 'NONE',  ( -3.250000000000014211, 7.362499999999993605, 3.980102097228917460E-16 ) ) ;
#9474 = ADVANCED_FACE ( 'NONE', ( #1364 ), #1209, .T. ) ;
#9475 = ORIENTED_EDGE ( 'NONE', *, *, #8006, .T. ) ;
#9476 = EDGE_LOOP ( 'NONE', ( #1854, #9431 ) ) ;
#9477 = CARTESIAN_POINT ( 'NONE',  ( -16.74999999999999289, -0.3152037684892597946, -22.25410949791978510 ) ) ;
#9478 = DIRECTION ( 'NONE',  ( 0.8660254037844383745, -0.5000000000000003331, 0.000000000000000000 ) ) ;
#9479 = VERTEX_POINT ( 'NONE', #10907 ) ;
#9480 = AXIS2_PLACEMENT_3D ( 'NONE', #14306, #11984, #100 ) ;
#9481 = CARTESIAN_POINT ( 'NONE',  ( -2.666008743340035902, -1.358588562373146624, -3.250302320816439217 ) ) ;
#9482 = VECTOR ( 'NONE', #6845, 1000.000000000000000 ) ;
#9483 = DIRECTION ( 'NONE',  ( 0.000000000000000000, 0.7547095802227716810, 0.6560590289905077199 ) ) ;
#9484 = DIRECTION ( 'NONE',  ( 0.000000000000000000, -1.000000000000000000, 0.000000000000000000 ) ) ;
#9485 = CIRCLE ( 'NONE', #6053, 2.500000000000002220 ) ;
#9486 = CARTESIAN_POINT ( 'NONE',  ( 11.10026251182900481, -11.00000029085427933, 69.17694817598119528 ) ) ;
#9487 = EDGE_CURVE ( 'NONE', #59, #11017, #11923, .T. ) ;
#9488 = CARTESIAN_POINT ( 'NONE',  ( 22.58164641901421632, 11.99999970914576863, -56.77834603255778489 ) ) ;
#9489 = VERTEX_POINT ( 'NONE', #8887 ) ;
#9490 = DIRECTION ( 'NONE',  ( 1.287488025362404182E-15, 1.000000000000000000, 0.000000000000000000 ) ) ;
#9491 = EDGE_CURVE ( 'NONE', #5205, #1380, #5238, .T. ) ;
#9492 = VECTOR ( 'NONE', #6902, 1000.000000000000000 ) ;
#9493 = CARTESIAN_POINT ( 'NONE',  ( -59.02799568714584666, 59.67411849586701322, -15.85886927678779834 ) ) ;
#9494 = VERTEX_POINT ( 'NONE', #8725 ) ;
#9495 = VECTOR ( 'NONE', #4622, 1000.000000000000000 ) ;
#9496 =( NAMED_UNIT ( * ) PLANE_ANGLE_UNIT ( ) SI_UNIT ( $, .RADIAN. ) );
#9497 = CARTESIAN_POINT ( 'NONE',  ( -0.7342670381812395064, -4.718750000000252243, 3.686397723581088304 ) ) ;
#9498 = ORIENTED_EDGE ( 'NONE', *, *, #14349, .F. ) ;
#9499 = CARTESIAN_POINT ( 'NONE',  ( -3.419120714393278249, -1.006874999999977760, -1.825951887684714503 ) ) ;
#9500 = CARTESIAN_POINT ( 'NONE',  ( -48.52438362644100067, 99.17411849586700612, -182.2484795835770228 ) ) ;
#9501 = TOROIDAL_SURFACE ( 'NONE', #1343, -1.151041666666720031, 4.401041666666736241 ) ;
#9502 = LINE ( 'NONE', #3771, #7336 ) ;
#9503 = EDGE_CURVE ( 'NONE', #1313, #9860, #12537, .T. ) ;
#9504 = DIRECTION ( 'NONE',  ( 0.000000000000000000, 0.000000000000000000, 1.000000000000000000 ) ) ;
#9505 = CARTESIAN_POINT ( 'NONE',  ( 57.41329019055577021, 5.000000000000001776, 101.4783111191910621 ) ) ;
#9506 = DIRECTION ( 'NONE',  ( -3.614007241618342978E-17, -1.000000000000000000, -0.000000000000000000 ) ) ;
#9507 = ADVANCED_FACE ( 'NONE', ( #1818 ), #6426, .F. ) ;
#9508 = CARTESIAN_POINT ( 'NONE',  ( -69.77438362644001302, 82.17411849586700612, -82.44847958357698303 ) ) ;
#9509 = VERTEX_POINT ( 'NONE', #3066 ) ;
#9510 = DIRECTION ( 'NONE',  ( 0.000000000000000000, 1.000000000000000000, 0.000000000000000000 ) ) ;
#9511 = VECTOR ( 'NONE', #1417, 999.9999999999998863 ) ;
#9512 = AXIS2_PLACEMENT_3D ( 'NONE', #721, #5469, #10167 ) ;
#9513 = ORIENTED_EDGE ( 'NONE', *, *, #1335, .F. ) ;
#9514 = LINE ( 'NONE', #13260, #8787 ) ;
#9515 = CARTESIAN_POINT ( 'NONE',  ( 3.503842902704710660, -2.631874999999911147, -1.061889326425361268 ) ) ;
#9516 = EDGE_LOOP ( 'NONE', ( #9936, #10792, #5009, #11626, #1028, #6546, #14498 ) ) ;
#9517 = ORIENTED_EDGE ( 'NONE', *, *, #12760, .T. ) ;
#9518 = EDGE_LOOP ( 'NONE', ( #13029, #8333, #7938, #6306 ) ) ;
#9519 = ADVANCED_FACE ( 'NONE', ( #12223 ), #3995, .F. ) ;
#9520 = LINE ( 'NONE', #9442, #13000 ) ;
#9521 = LINE ( 'NONE', #3712, #15011 ) ;
#9522 = EDGE_CURVE ( 'NONE', #9632, #11390, #12385, .T. ) ;
#9523 = CARTESIAN_POINT ( 'NONE',  ( -2.598076211353315124, -6.630110937211234507E-15, 4.500000000000000888 ) ) ;
#9524 = DIRECTION ( 'NONE',  ( -0.000000000000000000, -0.000000000000000000, 1.000000000000000000 ) ) ;
#9525 = AXIS2_PLACEMENT_3D ( 'NONE', #1103, #6012, #2490 ) ;
#9526 = LINE ( 'NONE', #8220, #5862 ) ;
#9527 = CARTESIAN_POINT ( 'NONE',  ( 0.6686498792469546260, -4.366249999999815223, 3.366016213005436075 ) ) ;
#9528 = ADVANCED_FACE ( 'NONE', ( #4305 ), #6655, .F. ) ;
#9529 = DIRECTION ( 'NONE',  ( 0.3469356515732558988, -0.9378889346118975956, 0.000000000000000000 ) ) ;
#9530 = EDGE_CURVE ( 'NONE', #5237, #5260, #2249, .T. ) ;
#9531 = ORIENTED_EDGE ( 'NONE', *, *, #12745, .T. ) ;
#9532 = FACE_OUTER_BOUND ( 'NONE', #9331, .T. ) ;
#9533 = ORIENTED_EDGE ( 'NONE', *, *, #10875, .F. ) ;
#9534 = ORIENTED_EDGE ( 'NONE', *, *, #7175, .T. ) ;
#9535 = ORIENTED_EDGE ( 'NONE', *, *, #12083, .T. ) ;
#9536 = AXIS2_PLACEMENT_3D ( 'NONE', #3997, #8727, #2839 ) ;
#9537 = SHAPE_REPRESENTATION_RELATIONSHIP ( 'NONE' , 'NONE' ,  #5010, #13674 ) ;
#9538 = CARTESIAN_POINT ( 'NONE',  ( -2.795825449145424191, -2.975624999999864517, -2.292747793747622609 ) ) ;
#9539 = DIRECTION ( 'NONE',  ( 1.000000000000000000, 0.000000000000000000, 0.000000000000000000 ) ) ;
#9540 = DIRECTION ( 'NONE',  ( 0.000000000000000000, -1.000000000000000000, 0.000000000000000000 ) ) ;
#9541 = FACE_OUTER_BOUND ( 'NONE', #12728, .T. ) ;
#9542 = DIRECTION ( 'NONE',  ( -0.08715574274766164919, -4.320305823558445788E-16, 0.9961946980917453232 ) ) ;
#9543 = DIRECTION ( 'NONE',  ( 0.000000000000000000, 0.000000000000000000, 1.000000000000000000 ) ) ;
#9544 = CARTESIAN_POINT ( 'NONE',  ( 1.581646419014216542, -11.40000029085424238, 0.2664120436859911956 ) ) ;
#9545 = STYLED_ITEM ( 'NONE', ( #9416 ), #418 ) ;
#9546 = CARTESIAN_POINT ( 'NONE',  ( -86.77438362644001302, 110.1741184958670061, -15.85886927678779834 ) ) ;
#9547 = DIRECTION ( 'NONE',  ( -1.000000000000000000, 0.000000000000000000, 0.000000000000000000 ) ) ;
#9548 = CARTESIAN_POINT ( 'NONE',  ( -55.52438362644000591, 65.17411849586700612, -152.4984795835769944 ) ) ;
#9549 = AXIS2_PLACEMENT_3D ( 'NONE', #4618, #12998, #2438 ) ;
#9550 = VERTEX_POINT ( 'NONE', #507 ) ;
#9551 = TOROIDAL_SURFACE ( 'NONE', #11066, 1.200000000000000178, 0.6000000000000000888 ) ;
#9552 = FACE_OUTER_BOUND ( 'NONE', #4908, .T. ) ;
#9553 = ORIENTED_EDGE ( 'NONE', *, *, #1919, .T. ) ;
#9554 = ORIENTED_EDGE ( 'NONE', *, *, #975, .F. ) ;
#9555 = ORIENTED_EDGE ( 'NONE', *, *, #11251, .F. ) ;
#9556 = DIRECTION ( 'NONE',  ( 0.08715574274766176022, 0.000000000000000000, -0.9961946980917453232 ) ) ;
#9557 = ORIENTED_EDGE ( 'NONE', *, *, #521, .F. ) ;
#9558 = VECTOR ( 'NONE', #5757, 1000.000000000000000 ) ;
#9559 = CARTESIAN_POINT ( 'NONE',  ( -4.185213075431162721, -1.499213562373157949, -0.001111502682336006596 ) ) ;
#9560 = CIRCLE ( 'NONE', #12557, 16.00000000000000000 ) ;
#9561 = TOROIDAL_SURFACE ( 'NONE', #4134, 2.093999815491831562, 0.2500000000000000000 ) ;
#9562 = CARTESIAN_POINT ( 'NONE',  ( -35.58670980944424400, 5.000000000000001776, 101.4783111191910621 ) ) ;
#9563 = CARTESIAN_POINT ( 'NONE',  ( 21.98164641901421135, 11.99999970914575975, -8.183940086454237317 ) ) ;
#9564 = DIRECTION ( 'NONE',  ( 0.000000000000000000, 0.000000000000000000, 1.000000000000000000 ) ) ;
#9565 = PRODUCT ( 'Self-Tapping Grease Fitting_8742T12', 'Self-Tapping Grease Fitting_8742T12', '', ( #5652 ) ) ;
#9566 = DIRECTION ( 'NONE',  ( 0.000000000000000000, 0.000000000000000000, -1.000000000000000000 ) ) ;
#9567 = ORIENTED_EDGE ( 'NONE', *, *, #5383, .F. ) ;
#9568 = CIRCLE ( 'NONE', #15022, 9.999999999999994671 ) ;
#9569 = CARTESIAN_POINT ( 'NONE',  ( -86.77438362644001302, 99.17411849586700612, -86.49847958357699440 ) ) ;
#9570 = CARTESIAN_POINT ( 'NONE',  ( 16.31442355444756132, 11.98691892176511331, 0.2637538782190264053 ) ) ;
#9571 = VECTOR ( 'NONE', #11561, 1000.000000000000000 ) ;
#9572 = ORIENTED_EDGE ( 'NONE', *, *, #9146, .T. ) ;
#9573 = CARTESIAN_POINT ( 'NONE',  ( 3.775473633219732505, -4.031249999999629630, -0.7524242524445519109 ) ) ;
#9574 = VERTEX_POINT ( 'NONE', #6493 ) ;
#9575 = EDGE_CURVE ( 'NONE', #3708, #6323, #7805, .T. ) ;
#9576 = AXIS2_PLACEMENT_3D ( 'NONE', #2347, #7100, #4687 ) ;
#9577 = DIRECTION ( 'NONE',  ( 0.000000000000000000, 0.000000000000000000, 1.000000000000000000 ) ) ;
#9578 = EDGE_CURVE ( 'NONE', #13840, #10484, #11366, .T. ) ;
#9579 = CARTESIAN_POINT ( 'NONE',  ( -69.77438362644001302, 82.17411849586700612, -81.84847958357698872 ) ) ;
#9580 = TOROIDAL_SURFACE ( 'NONE', #13326, 2.700000000000000178, 0.2000000000000000111 ) ;
#9581 = DIRECTION ( 'NONE',  ( 0.000000000000000000, 0.000000000000000000, 1.000000000000000000 ) ) ;
#9582 = CARTESIAN_POINT ( 'NONE',  ( -69.77438362644001302, 82.17411849586700612, -183.7533135795160320 ) ) ;
#9583 = CARTESIAN_POINT ( 'NONE',  ( -64.53565528768383786, 67.29799558322736175, -81.84847958357697451 ) ) ;
#9584 = CYLINDRICAL_SURFACE ( 'NONE', #1889, 1.785937500000001066 ) ;
#9585 = CARTESIAN_POINT ( 'NONE',  ( 23.25000000000000000, -10.00000000000000000, 27.00000000000000000 ) ) ;
#9586 = ORIENTED_EDGE ( 'NONE', *, *, #14000, .T. ) ;
#9587 = DIRECTION ( 'NONE',  ( 6.982962677686266711E-15, 6.579622859988665673E-30, 1.000000000000000000 ) ) ;
#9588 = ORIENTED_EDGE ( 'NONE', *, *, #4090, .T. ) ;
#9589 = AXIS2_PLACEMENT_3D ( 'NONE', #5701, #9164, #4595 ) ;
#9590 = DIRECTION ( 'NONE',  ( -0.000000000000000000, 0.000000000000000000, -1.000000000000000000 ) ) ;
#9591 = CARTESIAN_POINT ( 'NONE',  ( 3.535094671665901078, -3.584999999999991083, -0.001309597400350227814 ) ) ;
#9592 = EDGE_LOOP ( 'NONE', ( #14413, #1796, #3417, #2792 ) ) ;
#9593 = EDGE_CURVE ( 'NONE', #13931, #8947, #8452, .T. ) ;
#9594 = EDGE_LOOP ( 'NONE', ( #879, #7726 ) ) ;
#9595 = EDGE_CURVE ( 'NONE', #2658, #8154, #5745, .T. ) ;
#9596 = ORIENTED_EDGE ( 'NONE', *, *, #725, .F. ) ;
#9597 = FACE_OUTER_BOUND ( 'NONE', #3341, .T. ) ;
#9598 = CARTESIAN_POINT ( 'NONE',  ( -62.02799568714584666, 60.67411849586701322, -73.34256232478206528 ) ) ;
#9599 = CARTESIAN_POINT ( 'NONE',  ( -3.897114317029972685, -9.945166405816852549E-15, -2.249999999999999112 ) ) ;
#9600 =( REPRESENTATION_RELATIONSHIP ('NONE','NONE', #13541, #4448 ) REPRESENTATION_RELATIONSHIP_WITH_TRANSFORMATION ( #6568 )SHAPE_REPRESENTATION_RELATIONSHIP( ) );
#9601 = CIRCLE ( 'NONE', #2430, 0.5999999999999998668 ) ;
#9602 = DIRECTION ( 'NONE',  ( -1.000000000000000000, 0.000000000000000000, 0.000000000000000000 ) ) ;
#9603 = CARTESIAN_POINT ( 'NONE',  ( 15.50000000000000000, -0.2000000000000000111, -22.50000000000000000 ) ) ;
#9604 = CARTESIAN_POINT ( 'NONE',  ( -69.77438362644001302, 82.17411849586700612, -152.4984795835769944 ) ) ;
#9605 = CARTESIAN_POINT ( 'NONE',  ( 0.6849063648203621568, -3.803749999999915143, -3.438650935610223947 ) ) ;
#9606 = DIRECTION ( 'NONE',  ( 0.000000000000000000, 1.000000000000000000, 0.000000000000000000 ) ) ;
#9607 = ADVANCED_FACE ( 'NONE', ( #14775 ), #6245, .T. ) ;
#9608 = EDGE_LOOP ( 'NONE', ( #15029, #13640, #9763, #3679 ) ) ;
#9609 = EDGE_CURVE ( 'NONE', #14989, #9134, #12457, .T. ) ;
#9610 = DIRECTION ( 'NONE',  ( -0.000000000000000000, -0.000000000000000000, 1.000000000000000000 ) ) ;
#9611 = ORIENTED_EDGE ( 'NONE', *, *, #7216, .F. ) ;
#9612 = EDGE_LOOP ( 'NONE', ( #5677, #3434, #9937, #8171, #9227 ) ) ;
#9613 = VERTEX_POINT ( 'NONE', #5411 ) ;
#9614 = ORIENTED_EDGE ( 'NONE', *, *, #12843, .F. ) ;
#9615 = EDGE_CURVE ( 'NONE', #1401, #2251, #4230, .T. ) ;
#9616 = AXIS2_PLACEMENT_3D ( 'NONE', #10514, #3698, #7281 ) ;
#9617 = ADVANCED_FACE ( 'NONE', ( #657 ), #2751, .F. ) ;
#9618 = EDGE_CURVE ( 'NONE', #134, #455, #1273, .T. ) ;
#9619 = LINE ( 'NONE', #14352, #1362 ) ;
#9620 = DIRECTION ( 'NONE',  ( -0.9375000000000004441, 0.000000000000000000, -0.3479852726768752902 ) ) ;
#9621 = LINE ( 'NONE', #79, #10969 ) ;
#9622 = PLANE ( 'NONE',  #1136 ) ;
#9623 = PLANE ( 'NONE',  #3166 ) ;
#9624 = LINE ( 'NONE', #13290, #9511 ) ;
#9625 = CARTESIAN_POINT ( 'NONE',  ( -38.27438362644000591, 114.1741184958670061, -79.49847958357700861 ) ) ;
#9626 = CARTESIAN_POINT ( 'NONE',  ( -14.25000000000000000, -0.2038245569916330158, -21.77831216351300014 ) ) ;
#9627 = CARTESIAN_POINT ( 'NONE',  ( -16.75000000000000000, -0.2038245569916330158, -21.77831216351300014 ) ) ;
#9628 = VECTOR ( 'NONE', #3775, 1000.000000000000000 ) ;
#9629 = ADVANCED_FACE ( 'NONE', ( #15224 ), #4617, .F. ) ;
#9630 = ORIENTED_EDGE ( 'NONE', *, *, #2795, .T. ) ;
#9631 = CARTESIAN_POINT ( 'NONE',  ( -62.27438362644000591, 75.17411849586699191, -58.99847958357700151 ) ) ;
#9632 = VERTEX_POINT ( 'NONE', #4534 ) ;
#9633 = ORIENTED_EDGE ( 'NONE', *, *, #13699, .T. ) ;
#9634 = CYLINDRICAL_SURFACE ( 'NONE', #14651, 0.6000000000000000888 ) ;
#9635 = ADVANCED_FACE ( 'NONE', ( #882 ), #9175, .F. ) ;
#9636 = CARTESIAN_POINT ( 'NONE',  ( -0.4250114624646683659, -0.2656249999999867883, -4.327074173745135255 ) ) ;
#9637 = CARTESIAN_POINT ( 'NONE',  ( 0.8248545445007013921, -1.217963562373110653, -4.141066646055018730 ) ) ;
#9638 = CARTESIAN_POINT ( 'NONE',  ( -52.77438362643999881, 69.42411849586700612, -145.4984795835769944 ) ) ;
#9639 = CARTESIAN_POINT ( 'NONE',  ( -54.81638362644100226, 97.99516924618178848, -147.9984795835769944 ) ) ;
#9640 = DIRECTION ( 'NONE',  ( 1.000000000000000000, 0.000000000000000000, 0.000000000000000000 ) ) ;
#9641 = B_SPLINE_CURVE_WITH_KNOTS ( 'NONE', 3,
 ( #12589, #5302, #12513, #6630 ),
 .UNSPECIFIED., .F., .F.,
 ( 4, 4 ),
 ( 0.002598307151460994141, 0.005196383362814307842 ),
 .UNSPECIFIED. ) ;
#9642 = CYLINDRICAL_SURFACE ( 'NONE', #12723, 2.500000000000002220 ) ;
#9643 = CARTESIAN_POINT ( 'NONE',  ( -82.27438362643999881, 65.17411849586700612, -152.4984795835769944 ) ) ;
#9644 = ORIENTED_EDGE ( 'NONE', *, *, #12120, .F. ) ;
#9645 = CARTESIAN_POINT ( 'NONE',  ( 15.50000000000000000, -1.037157890325000054, 22.50000000000000000 ) ) ;
#9646 = ORIENTED_EDGE ( 'NONE', *, *, #7451, .T. ) ;
#9647 = SURFACE_STYLE_USAGE ( .BOTH. , #5011 ) ;
#9648 = CARTESIAN_POINT ( 'NONE',  ( -3.613419487966115895, -3.562500000000009326, 1.498272701152596031 ) ) ;
#9649 = ORIENTED_EDGE ( 'NONE', *, *, #11424, .T. ) ;
#9650 = CARTESIAN_POINT ( 'NONE',  ( -0.3809421545647762031, -0.8506249999999871969, -3.878187885777538035 ) ) ;
#9651 = DIRECTION ( 'NONE',  ( 0.000000000000000000, 1.000000000000000000, 0.000000000000000000 ) ) ;
#9652 = CARTESIAN_POINT ( 'NONE',  ( 22.58164641901421632, -3.579317323512964499, -0.3335879563140091153 ) ) ;
#9653 = CARTESIAN_POINT ( 'NONE',  ( 16.99691247867024657, 3.529302617095105621, 1.266532794505838000 ) ) ;
#9654 = PLANE ( 'NONE',  #10727 ) ;
#9655 = DIRECTION ( 'NONE',  ( 1.000000000000000000, 1.445602896647339163E-16, -0.000000000000000000 ) ) ;
#9656 = DIRECTION ( 'NONE',  ( -2.551930889570659960E-15, 1.000000000000000000, 0.000000000000000000 ) ) ;
#9657 = ORIENTED_EDGE ( 'NONE', *, *, #4607, .T. ) ;
#9658 = DIRECTION ( 'NONE',  ( 3.996802888650560011E-13, 1.000000000000000000, 0.000000000000000000 ) ) ;
#9659 = DIRECTION ( 'NONE',  ( 1.000000000000000000, 0.000000000000000000, 0.000000000000000000 ) ) ;
#9660 = EDGE_CURVE ( 'NONE', #215, #5825, #12909, .T. ) ;
#9661 = ORIENTED_EDGE ( 'NONE', *, *, #9898, .T. ) ;
#9662 = CARTESIAN_POINT ( 'NONE',  ( -35.58670980944424400, 0.000000000000000000, 129.5095611191910621 ) ) ;
#9663 = CARTESIAN_POINT ( 'NONE',  ( -0.3421672931279376995, -3.850625000000083009, -3.483230393025888105 ) ) ;
#9664 = ORIENTED_EDGE ( 'NONE', *, *, #9344, .T. ) ;
#9665 = ORIENTED_EDGE ( 'NONE', *, *, #14450, .F. ) ;
#9666 = ORIENTED_EDGE ( 'NONE', *, *, #10523, .F. ) ;
#9667 = B_SPLINE_CURVE_WITH_KNOTS ( 'NONE', 3,
 ( #3334, #13821, #7916, #8067, #15041, #12883 ),
 .UNSPECIFIED., .F., .F.,
 ( 4, 2, 4 ),
 ( 0.0002380763768129734448, 0.7291065797294589146, 1.457975083082104995 ),
 .UNSPECIFIED. ) ;
#9668 = DIRECTION ( 'NONE',  ( 0.7071067811865475727, 0.000000000000000000, -0.7071067811865475727 ) ) ;
#9669 = DIRECTION ( 'NONE',  ( -0.08715574274766131613, 0.000000000000000000, 0.9961946980917453232 ) ) ;
#9670 = DIRECTION ( 'NONE',  ( 1.000000000000000000, 0.000000000000000000, 0.000000000000000000 ) ) ;
#9671 = AXIS2_PLACEMENT_3D ( 'NONE', #14566, #4015, #12163 ) ;
#9672 = DIRECTION ( 'NONE',  ( -1.000000000000000000, 1.287488025362404182E-15, 0.000000000000000000 ) ) ;
#9673 = CYLINDRICAL_SURFACE ( 'NONE', #12959, 1.000000000000000888 ) ;
#9674 = PLANE ( 'NONE',  #9294 ) ;
#9675 = EDGE_CURVE ( 'NONE', #11390, #3042, #8708, .T. ) ;
#9676 = CARTESIAN_POINT ( 'NONE',  ( -2.894177851434075244, -3.991249999999941789, -1.934899151906914305 ) ) ;
#9677 = DIRECTION ( 'NONE',  ( 1.000000000000000000, 0.000000000000000000, 0.000000000000000000 ) ) ;
#9678 = EDGE_LOOP ( 'NONE', ( #13030, #5638, #4027, #14272, #4437, #9649 ) ) ;
#9679 = DIRECTION ( 'NONE',  ( 1.000000000000000000, 0.000000000000000000, 0.000000000000000000 ) ) ;
#9680 = EDGE_CURVE ( 'NONE', #1533, #3437, #5878, .T. ) ;
#9681 = VERTEX_POINT ( 'NONE', #9258 ) ;
#9682 = AXIS2_PLACEMENT_3D ( 'NONE', #7260, #11985, #15147 ) ;
#9683 = ORIENTED_EDGE ( 'NONE', *, *, #8558, .F. ) ;
#9684 = ORIENTED_EDGE ( 'NONE', *, *, #448, .F. ) ;
#9685 = EDGE_LOOP ( 'NONE', ( #6020, #7637, #3058, #1218 ) ) ;
#9686 = AXIS2_PLACEMENT_3D ( 'NONE', #12365, #6476, #560 ) ;
#9687 = DIRECTION ( 'NONE',  ( 0.000000000000000000, 0.000000000000000000, -1.000000000000000000 ) ) ;
#9688 = CARTESIAN_POINT ( 'NONE',  ( -1.038475776471825762, -3.288125000000012843, 3.420226703972062854 ) ) ;
#9689 = SURFACE_SIDE_STYLE ('',( #4978 ) ) ;
#9690 = DIRECTION ( 'NONE',  ( 0.000000000000000000, 0.000000000000000000, -1.000000000000000000 ) ) ;
#9691 = CARTESIAN_POINT ( 'NONE',  ( -52.77438362644100067, 101.5320169952374414, -150.4984795835770228 ) ) ;
#9692 = CARTESIAN_POINT ( 'NONE',  ( -1.629699455448989389E-14, 8.699999999999999289, 5.655858585055787181E-29 ) ) ;
#9693 = VECTOR ( 'NONE', #10579, 1000.000000000000114 ) ;
#9694 = DIRECTION ( 'NONE',  ( 1.000000000000000000, 0.000000000000000000, 0.000000000000000000 ) ) ;
#9695 = CARTESIAN_POINT ( 'NONE',  ( 1.634139617129772404, -85.69524470659700910, -0.3335879563140516924 ) ) ;
#9696 = LINE ( 'NONE', #5148, #4588 ) ;
#9697 = ADVANCED_FACE ( 'NONE', ( #15302 ), #5008, .T. ) ;
#9698 = CARTESIAN_POINT ( 'NONE',  ( -14.45366306705349224, -0.2717122460102528447, -21.66072723692568402 ) ) ;
#9699 = CARTESIAN_POINT ( 'NONE',  ( 16.74999999999999289, -0.3152037684892571301, -22.74589050208021845 ) ) ;
#9700 = ORIENTED_EDGE ( 'NONE', *, *, #13848, .T. ) ;
#9701 = DIRECTION ( 'NONE',  ( 0.000000000000000000, 0.000000000000000000, -1.000000000000000000 ) ) ;
#9702 = AXIS2_PLACEMENT_3D ( 'NONE', #515, #4170, #12394 ) ;
#9703 = EDGE_CURVE ( 'NONE', #10484, #6998, #12839, .T. ) ;
#9704 = VERTEX_POINT ( 'NONE', #9337 ) ;
#9705 = EDGE_CURVE ( 'NONE', #11017, #6230, #3019, .T. ) ;
#9706 = ORIENTED_EDGE ( 'NONE', *, *, #13248, .T. ) ;
#9707 = CARTESIAN_POINT ( 'NONE',  ( -2.933994605034233150, -5.163125000000027498, 1.567297863280187054 ) ) ;
#9708 = AXIS2_PLACEMENT_3D ( 'NONE', #13064, #10799, #9620 ) ;
#9709 = CARTESIAN_POINT ( 'NONE',  ( -4.359283389060221836, 0.4687500000000111022, 0.8687415714326495175 ) ) ;
#9710 = CARTESIAN_POINT ( 'NONE',  ( -3.999387421850409741, -1.546088562373119979, 1.212041425752152568 ) ) ;
#9711 = AXIS2_PLACEMENT_3D ( 'NONE', #11603, #1981, #8114 ) ;
#9712 = EDGE_CURVE ( 'NONE', #11163, #1167, #10344, .T. ) ;
#9713 = DIRECTION ( 'NONE',  ( 0.000000000000000000, -1.000000000000000000, 0.000000000000000000 ) ) ;
#9714 = DIRECTION ( 'NONE',  ( 0.000000000000000000, 0.000000000000000000, 1.000000000000000000 ) ) ;
#9715 = CONICAL_SURFACE ( 'NONE', #5777, 4.500000000000000888, 0.7853981633974500554 ) ;
#9716 = FACE_OUTER_BOUND ( 'NONE', #9250, .T. ) ;
#9717 = CARTESIAN_POINT ( 'NONE',  ( -69.77438362644001302, 82.17411849586700612, -83.44847958357698303 ) ) ;
#9718 = EDGE_CURVE ( 'NONE', #2194, #4503, #10937, .T. ) ;
#9719 = AXIS2_PLACEMENT_3D ( 'NONE', #359, #6132, #5106 ) ;
#9720 = DIRECTION ( 'NONE',  ( 0.000000000000000000, 0.000000000000000000, 1.000000000000000000 ) ) ;
#9721 = ORIENTED_EDGE ( 'NONE', *, *, #2088, .T. ) ;
#9722 = CARTESIAN_POINT ( 'NONE',  ( -65.90140028023573393, 75.17411849586525818, -29.37106258560738681 ) ) ;
#9723 = ADVANCED_FACE ( 'NONE', ( #1034, #13771 ), #12612, .F. ) ;
#9724 = EDGE_CURVE ( 'NONE', #160, #2409, #13913, .T. ) ;
#9725 = VECTOR ( 'NONE', #4494, 1000.000000000000000 ) ;
#9726 = ORIENTED_EDGE ( 'NONE', *, *, #8935, .T. ) ;
#9727 =( NAMED_UNIT ( * ) SI_UNIT ( $, .STERADIAN. ) SOLID_ANGLE_UNIT ( ) );
#9728 = CARTESIAN_POINT ( 'NONE',  ( 3.389018004338130385, -4.078125000000095035, -1.813062472674689340 ) ) ;
#9729 = ORIENTED_EDGE ( 'NONE', *, *, #6965, .T. ) ;
#9730 = CARTESIAN_POINT ( 'NONE',  ( 3.568345045357413703, -3.936713562373220565, 1.479150544514123089 ) ) ;
#9731 = AXIS2_PLACEMENT_3D ( 'NONE', #9583, #14321, #8588 ) ;
#9732 = CARTESIAN_POINT ( 'NONE',  ( 2.697785604507370483, -1.459999999999946008, 2.699193867783821865 ) ) ;
#9733 = DIRECTION ( 'NONE',  ( 0.000000000000000000, -1.000000000000000000, 0.000000000000000000 ) ) ;
#9734 = CARTESIAN_POINT ( 'NONE',  ( -69.77438362644001302, 82.17411849586700612, -150.4984795835769944 ) ) ;
#9735 = AXIS2_PLACEMENT_3D ( 'NONE', #1349, #1268, #13155 ) ;
#9736 = CARTESIAN_POINT ( 'NONE',  ( -35.58670980944424400, 2.488961461112888074, 99.29549861919106490 ) ) ;
#9737 = CIRCLE ( 'NONE', #6780, 2.042000000000002036 ) ;
#9738 = CARTESIAN_POINT ( 'NONE',  ( -63.06767964790545022, 68.65632084656354550, -81.84847958357697451 ) ) ;
#9739 = CARTESIAN_POINT ( 'NONE',  ( 3.138279930143428764, -5.305558064392307038, 1.406575084002399612 ) ) ;
#9740 = CARTESIAN_POINT ( 'NONE',  ( -86.77438362644001302, 65.17411849586700612, -152.4984795835769944 ) ) ;
#9741 = CARTESIAN_POINT ( 'NONE',  ( -50.73238362643999722, 63.99516924618178848, -147.9984795835769944 ) ) ;
#9742 = CIRCLE ( 'NONE', #13472, 0.8000000000000113687 ) ;
#9743 = ORIENTED_EDGE ( 'NONE', *, *, #8874, .T. ) ;
#9744 = DIRECTION ( 'NONE',  ( 0.000000000000000000, 0.000000000000000000, -1.000000000000000000 ) ) ;
#9745 = ORIENTED_EDGE ( 'NONE', *, *, #2627, .F. ) ;
#9746 = CARTESIAN_POINT ( 'NONE',  ( -62.02799568714584666, 0.000000000000000000, -73.34256232478206528 ) ) ;
#9747 = CARTESIAN_POINT ( 'NONE',  ( 2.950365215318708323, -3.491249999999835651, 1.969791294043586660 ) ) ;
#9748 = EDGE_LOOP ( 'NONE', ( #3915, #2327, #8310, #9918 ) ) ;
#9749 = ORIENTED_EDGE ( 'NONE', *, *, #11349, .F. ) ;
#9750 = AXIS2_PLACEMENT_3D ( 'NONE', #6861, #3588, #11581 ) ;
#9751 = DIRECTION ( 'NONE',  ( 0.000000000000000000, 0.000000000000000000, -1.000000000000000000 ) ) ;
#9752 = CARTESIAN_POINT ( 'NONE',  ( -13.41835358098578723, -2.908542394189813650E-07, 0.2664120436859911956 ) ) ;
#9753 = DIRECTION ( 'NONE',  ( 1.000000000000000000, -0.000000000000000000, 0.000000000000000000 ) ) ;
#9754 = CARTESIAN_POINT ( 'NONE',  ( 15.08565937784311117, -0.3156604612129180754, -21.29584399676446793 ) ) ;
#9755 = CARTESIAN_POINT ( 'NONE',  ( -15.50000000000000000, -0.4000000000005236034, -25.79999999999947136 ) ) ;
#9756 = AXIS2_PLACEMENT_3D ( 'NONE', #1228, #13116, #2464 ) ;
#9757 = VECTOR ( 'NONE', #12858, 1000.000000000000000 ) ;
#9758 = DIRECTION ( 'NONE',  ( -0.000000000000000000, -0.000000000000000000, 1.000000000000000000 ) ) ;
#9759 = ORIENTED_EDGE ( 'NONE', *, *, #3722, .T. ) ;
#9760 = CARTESIAN_POINT ( 'NONE',  ( -52.77438362644000591, 65.17411849586700612, -152.4984795835769944 ) ) ;
#9761 = ORIENTED_EDGE ( 'NONE', *, *, #10162, .F. ) ;
#9762 = ORIENTED_EDGE ( 'NONE', *, *, #4338, .T. ) ;
#9763 = ORIENTED_EDGE ( 'NONE', *, *, #5673, .F. ) ;
#9764 = ORIENTED_EDGE ( 'NONE', *, *, #14428, .F. ) ;
#9765 = DIRECTION ( 'NONE',  ( 0.000000000000000000, 0.000000000000000000, -1.000000000000000000 ) ) ;
#9766 = EDGE_CURVE ( 'NONE', #11761, #4585, #13847, .T. ) ;
#9767 = CARTESIAN_POINT ( 'NONE',  ( 2.674095735623811088, -1.709999999999972209, -2.676057788957662886 ) ) ;
#9768 = CIRCLE ( 'NONE', #15214, 2.500000000000002220 ) ;
#9769 = DIRECTION ( 'NONE',  ( -1.000000000000000000, 0.000000000000000000, 0.000000000000000000 ) ) ;
#9770 = CARTESIAN_POINT ( 'NONE',  ( 2.736090332400194836, -3.875000000000003553, 2.737522629006357455 ) ) ;
#9771 = DIRECTION ( 'NONE',  ( 0.000000000000000000, 0.000000000000000000, 1.000000000000000000 ) ) ;
#9772 = EDGE_CURVE ( 'NONE', #5866, #13359, #12679, .T. ) ;
#9773 = DIRECTION ( 'NONE',  ( -1.000000000000000000, 0.000000000000000000, 0.000000000000000000 ) ) ;
#9774 = CARTESIAN_POINT ( 'NONE',  ( -69.77438362644001302, 82.17411849586700612, -82.44847958357698303 ) ) ;
#9775 = CARTESIAN_POINT ( 'NONE',  ( -69.77438362644001302, 82.17411849586700612, -79.59847958357700293 ) ) ;
#9776 = FACE_OUTER_BOUND ( 'NONE', #4707, .T. ) ;
#9777 = FACE_OUTER_BOUND ( 'NONE', #9800, .T. ) ;
#9778 = FACE_OUTER_BOUND ( 'NONE', #1165, .T. ) ;
#9779 = VERTEX_POINT ( 'NONE', #11518 ) ;
#9780 = DIRECTION ( 'NONE',  ( 1.000000000000000000, 0.000000000000000000, 0.000000000000000000 ) ) ;
#9781 = VECTOR ( 'NONE', #9268, 1000.000000000000000 ) ;
#9782 = ORIENTED_EDGE ( 'NONE', *, *, #3186, .F. ) ;
#9783 = AXIS2_PLACEMENT_3D ( 'NONE', #5177, #1819, #9885 ) ;
#9784 = ORIENTED_EDGE ( 'NONE', *, *, #4504, .T. ) ;
#9785 = AXIS2_PLACEMENT_3D ( 'NONE', #2570, #10639, #8241 ) ;
#9786 = UNCERTAINTY_MEASURE_WITH_UNIT (LENGTH_MEASURE( 1.000000000000000082E-05 ), #5290, 'distance_accuracy_value', 'NONE');
#9787 = CARTESIAN_POINT ( 'NONE',  ( 2.063655046872799659, -5.725624999999673115, -2.513280214060439999 ) ) ;
#9788 = LINE ( 'NONE', #14521, #9443 ) ;
#9789 = EDGE_CURVE ( 'NONE', #5891, #1706, #31, .T. ) ;
#9790 = CARTESIAN_POINT ( 'NONE',  ( -1.287538504858034338, -4.897500000000167830, -3.105113058795574421 ) ) ;
#9791 = DIRECTION ( 'NONE',  ( 0.000000000000000000, 0.000000000000000000, -1.000000000000000000 ) ) ;
#9792 = CIRCLE ( 'NONE', #1630, 0.1999999999999987899 ) ;
#9793 = DIRECTION ( 'NONE',  ( 0.000000000000000000, 0.000000000000000000, -1.000000000000000000 ) ) ;
#9794 = ADVANCED_FACE ( 'NONE', ( #8102 ), #2203, .F. ) ;
#9795 = CARTESIAN_POINT ( 'NONE',  ( 15.29686605390242526, -0.2715358723600077018, -23.82609623451301317 ) ) ;
#9796 = CIRCLE ( 'NONE', #9549, 11.49999999999999645 ) ;
#9797 = CARTESIAN_POINT ( 'NONE',  ( -96.77438362643999881, 59.67411849586700612, -79.59847958357700293 ) ) ;
#9798 = AXIS2_PLACEMENT_3D ( 'NONE', #3485, #5993, #66 ) ;
#9799 = DIRECTION ( 'NONE',  ( 1.000000000000000000, -0.000000000000000000, 0.000000000000000000 ) ) ;
#9800 = EDGE_LOOP ( 'NONE', ( #3601, #14672, #2718, #13825, #5572 ) ) ;
#9801 = DIRECTION ( 'NONE',  ( 0.000000000000000000, -1.000000000000000000, 0.000000000000000000 ) ) ;
#9802 = EDGE_CURVE ( 'NONE', #4608, #215, #9941, .T. ) ;
#9803 = ADVANCED_FACE ( 'NONE', ( #7109 ), #13226, .F. ) ;
#9804 = ORIENTED_EDGE ( 'NONE', *, *, #12867, .T. ) ;
#9805 = CIRCLE ( 'NONE', #6130, 2.000000000000001776 ) ;
#9806 = SPHERICAL_SURFACE ( 'NONE', #11296, 0.8600000000000014300 ) ;
#9807 = CARTESIAN_POINT ( 'NONE',  ( -1.185531852251327400, -2.296875000000050182, -3.903075577084617720 ) ) ;
#9808 = ORIENTED_EDGE ( 'NONE', *, *, #9886, .T. ) ;
#9809 = VECTOR ( 'NONE', #252, 1000.000000000000000 ) ;
#9810 = EDGE_CURVE ( 'NONE', #14624, #726, #5954, .T. ) ;
#9811 = CARTESIAN_POINT ( 'NONE',  ( 0.0009559351216548812522, -5.249213562373182818, -3.689142743541748093 ) ) ;
#9812 = FACE_OUTER_BOUND ( 'NONE', #3337, .T. ) ;
#9813 = ADVANCED_FACE ( 'NONE', ( #10651 ), #2669, .F. ) ;
#9814 = FACE_OUTER_BOUND ( 'NONE', #2517, .T. ) ;
#9815 = EDGE_CURVE ( 'NONE', #10442, #4229, #2476, .T. ) ;
#9816 = DIRECTION ( 'NONE',  ( 0.000000000000000000, 1.000000000000000000, 0.000000000000000000 ) ) ;
#9817 = CIRCLE ( 'NONE', #6855, 1.999999999999986233 ) ;
#9818 = CARTESIAN_POINT ( 'NONE',  ( 16.99691247867024657, -3.779330867977714892, 1.266532794505838000 ) ) ;
#9819 = AXIS2_PLACEMENT_3D ( 'NONE', #7982, #6539, #14811 ) ;
#9820 = CARTESIAN_POINT ( 'NONE',  ( -77.52077156573416516, 103.6741184958669777, -73.34256232478206528 ) ) ;
#9821 = CARTESIAN_POINT ( 'NONE',  ( 2.621470655598105548, -5.354113571045281184, 2.112355036808595710 ) ) ;
#9822 = PLANE ( 'NONE',  #4372 ) ;
#9823 = CARTESIAN_POINT ( 'NONE',  ( -52.77438362644000591, 65.17411849586700612, -145.4984795835769660 ) ) ;
#9824 = DIRECTION ( 'NONE',  ( -0.4999999999999998890, 0.8660254037844387076, 0.000000000000000000 ) ) ;
#9825 = ORIENTED_EDGE ( 'NONE', *, *, #15220, .T. ) ;
#9826 = ORIENTED_EDGE ( 'NONE', *, *, #13985, .T. ) ;
#9827 = ORIENTED_EDGE ( 'NONE', *, *, #1709, .F. ) ;
#9828 = CARTESIAN_POINT ( 'NONE',  ( 9.531855622864829864E-16, 8.384405323238834029, 0.000000000000000000 ) ) ;
#9829 = CARTESIAN_POINT ( 'NONE',  ( 2.743301530724825188, -3.475625000000028386, 2.252549412313518573 ) ) ;
#9830 = ORIENTED_EDGE ( 'NONE', *, *, #12957, .F. ) ;
#9831 = VECTOR ( 'NONE', #4773, 999.9999999999998863 ) ;
#9832 = ORIENTED_EDGE ( 'NONE', *, *, #5074, .F. ) ;
#9833 = EDGE_CURVE ( 'NONE', #1912, #4210, #14399, .T. ) ;
#9834 = LINE ( 'NONE', #1465, #11666 ) ;
#9835 = CARTESIAN_POINT ( 'NONE',  ( -86.77438362644001302, 110.1741184958670061, -15.85886927678779834 ) ) ;
#9836 = CARTESIAN_POINT ( 'NONE',  ( -35.58670980944424400, 2.488961461112888074, 127.7236236191910734 ) ) ;
#9837 = FACE_OUTER_BOUND ( 'NONE', #6530, .T. ) ;
#9838 = PLANE ( 'NONE',  #5113 ) ;
#9839 = DIRECTION ( 'NONE',  ( 0.000000000000000000, 1.000000000000000000, 0.000000000000000000 ) ) ;
#9840 = VECTOR ( 'NONE', #13611, 1000.000000000000114 ) ;
#9841 = ORIENTED_EDGE ( 'NONE', *, *, #2304, .F. ) ;
#9842 = LINE ( 'NONE', #1701, #7044 ) ;
#9843 = EDGE_LOOP ( 'NONE', ( #5711, #13669 ) ) ;
#9844 = ORIENTED_EDGE ( 'NONE', *, *, #11625, .F. ) ;
#9845 = VERTEX_POINT ( 'NONE', #13153 ) ;
#9846 = VERTEX_POINT ( 'NONE', #10735 ) ;
#9847 = VERTEX_POINT ( 'NONE', #7413 ) ;
#9848 =( BOUNDED_CURVE ( )  B_SPLINE_CURVE ( 3, ( #15150, #11602, #1042, #10351 ),
 .UNSPECIFIED., .F., .T. ) 
 B_SPLINE_CURVE_WITH_KNOTS ( ( 4, 4 ),
 ( 0.000000000000000000, 0.08794004307218132588 ),
 .UNSPECIFIED. ) 
 CURVE ( )  GEOMETRIC_REPRESENTATION_ITEM ( )  RATIONAL_B_SPLINE_CURVE ( ( 1.000000000000000000, 0.9993556495590054656, 0.9993556495590054656, 1.000000000000000000 ) ) 
 REPRESENTATION_ITEM ( '' )  );
#9849 = CARTESIAN_POINT ( 'NONE',  ( -57.27438362644000591, 65.17411849586700612, -145.4984795835769660 ) ) ;
#9850 = CARTESIAN_POINT ( 'NONE',  ( 3.341236413112389947, -1.663124999999897824, -1.787503410618120459 ) ) ;
#9851 = AXIS2_PLACEMENT_3D ( 'NONE', #5774, #6711, #9093 ) ;
#9852 = CARTESIAN_POINT ( 'NONE',  ( -3.745604523531179897, -3.546874999999923173, 1.135144126415479793 ) ) ;
#9853 = CARTESIAN_POINT ( 'NONE',  ( -64.53565528768383786, 67.29799558322736175, -83.44847958357698303 ) ) ;
#9854 = DIRECTION ( 'NONE',  ( 6.982962677686266711E-15, 6.579622859988665673E-30, 1.000000000000000000 ) ) ;
#9855 = CARTESIAN_POINT ( 'NONE',  ( -63.28565528768381654, 67.29799558322736175, -83.44847958357698303 ) ) ;
#9856 = FACE_OUTER_BOUND ( 'NONE', #1811, .T. ) ;
#9857 = CARTESIAN_POINT ( 'NONE',  ( -69.77438362644001302, 82.17411849586700612, -69.19783113114588957 ) ) ;
#9858 = CARTESIAN_POINT ( 'NONE',  ( -84.73238362644100619, 100.3530677455522238, -147.9984795835769944 ) ) ;
#9859 = CARTESIAN_POINT ( 'NONE',  ( 21.98164641901421135, 3.654316742536408924, 0.2664120436859909735 ) ) ;
#9860 = VERTEX_POINT ( 'NONE', #4695 ) ;
#9861 = DIRECTION ( 'NONE',  ( 1.000000000000000000, 0.000000000000000000, 0.000000000000000000 ) ) ;
#9862 = EDGE_LOOP ( 'NONE', ( #10136, #14594, #15020, #7834 ) ) ;
#9863 = AXIS2_PLACEMENT_3D ( 'NONE', #2801, #479, #7554 ) ;
#9864 = ORIENTED_EDGE ( 'NONE', *, *, #11799, .T. ) ;
#9865 = EDGE_LOOP ( 'NONE', ( #5365, #3242, #1548, #10332 ) ) ;
#9866 = CARTESIAN_POINT ( 'NONE',  ( 2.894038744318182310, -5.506874999999972431, 1.545501402921559908 ) ) ;
#9867 = ADVANCED_FACE ( 'NONE', ( #12136 ), #8342, .T. ) ;
#9868 = DIRECTION ( 'NONE',  ( -2.345198365613508922E-35, -1.000000000000000000, -4.336808689942017736E-16 ) ) ;
#9869 = CARTESIAN_POINT ( 'NONE',  ( -3.322613055092911161, -5.069375000000116316, -0.3280989749989032256 ) ) ;
#9870 = CARTESIAN_POINT ( 'NONE',  ( -23.25000000000000000, -10.00000000000000000, -27.00000000000000000 ) ) ;
#9871 = DIRECTION ( 'NONE',  ( -1.000000000000000000, 0.000000000000000000, 0.000000000000000000 ) ) ;
#9872 = CARTESIAN_POINT ( 'NONE',  ( 14.25000000000000000, -2.500000000000000000, 21.77831216351300014 ) ) ;
#9873 = AXIS2_PLACEMENT_3D ( 'NONE', #8978, #12781, #6896 ) ;
#9874 = LINE ( 'NONE', #7574, #12593 ) ;
#9875 = CARTESIAN_POINT ( 'NONE',  ( -69.77438362644001302, 90.17411849586700612, -112.9984795835769944 ) ) ;
#9876 = CARTESIAN_POINT ( 'NONE',  ( 22.58164641901421632, 11.39999970914575833, 0.2664120436859911956 ) ) ;
#9877 = ORIENTED_EDGE ( 'NONE', *, *, #11709, .T. ) ;
#9878 = ORIENTED_CLOSED_SHELL ( 'NONE', *, #10003, .F. );
#9879 = LINE ( 'NONE', #259, #415 ) ;
#9880 = ADVANCED_FACE ( 'NONE', ( #12997 ), #6009, .F. ) ;
#9881 = ORIENTED_EDGE ( 'NONE', *, *, #4951, .F. ) ;
#9882 = ADVANCED_FACE ( 'NONE', ( #14373 ), #4850, .T. ) ;
#9883 = CARTESIAN_POINT ( 'NONE',  ( 3.935506471057187206, -2.046874999999910738, -1.192685225358429912 ) ) ;
#9884 = ORIENTED_EDGE ( 'NONE', *, *, #5180, .F. ) ;
#9885 = DIRECTION ( 'NONE',  ( 0.000000000000000000, -0.000000000000000000, -1.000000000000000000 ) ) ;
#9886 = EDGE_CURVE ( 'NONE', #7919, #6631, #3762, .T. ) ;
#9887 = DIRECTION ( 'NONE',  ( 0.9961946980917452121, -3.779777825264101491E-17, 0.08715574274766160756 ) ) ;
#9888 = DIRECTION ( 'NONE',  ( -0.000000000000000000, 1.000000000000000000, -0.000000000000000000 ) ) ;
#9889 = DIRECTION ( 'NONE',  ( 0.000000000000000000, 0.000000000000000000, -1.000000000000000000 ) ) ;
#9890 = DIRECTION ( 'NONE',  ( -1.000000000000000000, 0.000000000000000000, 0.000000000000000000 ) ) ;
#9891 = DIRECTION ( 'NONE',  ( -0.08715574274766155205, 0.000000000000000000, 0.9961946980917452121 ) ) ;
#9892 = DIRECTION ( 'NONE',  ( 0.000000000000000000, 1.000000000000000000, 0.000000000000000000 ) ) ;
#9893 = EDGE_CURVE ( 'NONE', #4480, #13685, #2504, .T. ) ;
#9894 = DIRECTION ( 'NONE',  ( 0.000000000000000000, 0.000000000000000000, -1.000000000000000000 ) ) ;
#9895 = ORIENTED_EDGE ( 'NONE', *, *, #3448, .T. ) ;
#9896 =( LENGTH_UNIT ( ) NAMED_UNIT ( * ) SI_UNIT ( .MILLI., .METRE. ) );
#9897 = ORIENTED_EDGE ( 'NONE', *, *, #8948, .T. ) ;
#9898 = EDGE_CURVE ( 'NONE', #3399, #4506, #4768, .T. ) ;
#9899 = APPLICATION_CONTEXT ( 'automotive_design' ) ;
#9900 = LINE ( 'NONE', #10123, #2599 ) ;
#9901 = EDGE_CURVE ( 'NONE', #14906, #1551, #11434, .T. ) ;
#9902 = CARTESIAN_POINT ( 'NONE',  ( -2.135074830120813782, -1.241249999999904707, 3.197897516496418735 ) ) ;
#9903 = ORIENTED_EDGE ( 'NONE', *, *, #11212, .F. ) ;
#9904 = CARTESIAN_POINT ( 'NONE',  ( 11.10026251182900303, 10.99999970914572600, 69.17694817598120949 ) ) ;
#9905 = PRODUCT_DEFINITION_SHAPE ( 'NONE', 'NONE',  #15341 ) ;
#9906 = EDGE_CURVE ( 'NONE', #15133, #8823, #6108, .T. ) ;
#9907 = CARTESIAN_POINT ( 'NONE',  ( 1.787440017715160590, -5.131417235833041879, -3.208234933698080660 ) ) ;
#9908 = LINE ( 'NONE', #13266, #5073 ) ;
#9909 = DIRECTION ( 'NONE',  ( -2.551930889570659960E-15, 1.000000000000000000, 0.000000000000000000 ) ) ;
#9910 = FILL_AREA_STYLE_COLOUR ( '', #14907 ) ;
#9911 = CARTESIAN_POINT ( 'NONE',  ( -89.47438362643998744, 65.17411849586700612, -145.4984795835769944 ) ) ;
#9912 = ADVANCED_FACE ( 'NONE', ( #6187 ), #253, .F. ) ;
#9913 = CYLINDRICAL_SURFACE ( 'NONE', #1071, 1.999999999999988010 ) ;
#9914 = VERTEX_POINT ( 'NONE', #3835 ) ;
#9915 = CARTESIAN_POINT ( 'NONE',  ( -15.29686605391142606, -0.2715358723588648937, 23.82609623451821079 ) ) ;
#9916 = VERTEX_POINT ( 'NONE', #14600 ) ;
#9917 = ORIENTED_EDGE ( 'NONE', *, *, #12700, .F. ) ;
#9918 = ORIENTED_EDGE ( 'NONE', *, *, #8021, .F. ) ;
#9919 = ORIENTED_EDGE ( 'NONE', *, *, #11915, .F. ) ;
#9920 = EDGE_LOOP ( 'NONE', ( #13687, #7869, #5129 ) ) ;
#9921 = CARTESIAN_POINT ( 'NONE',  ( -84.73238362643999722, 63.99516924618178848, -147.9984795835769944 ) ) ;
#9922 = CARTESIAN_POINT ( 'NONE',  ( 3.601230736643932673, -2.553749999999958220, 0.7149504581460995878 ) ) ;
#9923 = DIRECTION ( 'NONE',  ( -1.000000000000000000, 0.000000000000000000, 0.000000000000000000 ) ) ;
#9924 = CARTESIAN_POINT ( 'NONE',  ( -3.249648180954406662, -3.593749999999990230, 2.170113394669044293 ) ) ;
#9925 = CARTESIAN_POINT ( 'NONE',  ( -16.75000000000000000, -0.2038245569916330158, 21.77831216351300014 ) ) ;
#9926 = CARTESIAN_POINT ( 'NONE',  ( -86.77438362644001302, 65.17411849586700612, -79.59847958357700293 ) ) ;
#9927 = DIRECTION ( 'NONE',  ( 0.000000000000000000, 0.000000000000000000, -1.000000000000000000 ) ) ;
#9928 = CARTESIAN_POINT ( 'NONE',  ( 11.02010870769206541, 10.99999970914572600, 70.09311034953165631 ) ) ;
#9929 = CARTESIAN_POINT ( 'NONE',  ( 17.23697745638123280, 3.691760653673249681, -0.03314156585704653574 ) ) ;
#9930 = DIRECTION ( 'NONE',  ( -1.000000000000000000, -2.548822376660340629E-15, 0.000000000000000000 ) ) ;
#9931 = CARTESIAN_POINT ( 'NONE',  ( 16.75000000000000000, -0.3156864504677172611, -22.25638000318208398 ) ) ;
#9932 = ORIENTED_EDGE ( 'NONE', *, *, #5754, .F. ) ;
#9933 = CARTESIAN_POINT ( 'NONE',  ( -13.41835358098578723, 11.39999970914575833, 0.2664120436859911956 ) ) ;
#9934 = ORIENTED_EDGE ( 'NONE', *, *, #8878, .T. ) ;
#9935 = CIRCLE ( 'NONE', #7218, 17.85000000000000497 ) ;
#9936 = ORIENTED_EDGE ( 'NONE', *, *, #13797, .T. ) ;
#9937 = ORIENTED_EDGE ( 'NONE', *, *, #10743, .T. ) ;
#9938 = UNCERTAINTY_MEASURE_WITH_UNIT (LENGTH_MEASURE( 1.000000000000000082E-05 ), #4952, 'distance_accuracy_value', 'NONE');
#9939 = CARTESIAN_POINT ( 'NONE',  ( -2.129528971937844961, -4.944374999999755715, -2.592863122870769921 ) ) ;
#9940 = LINE ( 'NONE', #14755, #8456 ) ;
#9941 = CIRCLE ( 'NONE', #10431, 4.000000000000001776 ) ;
#9942 = CARTESIAN_POINT ( 'NONE',  ( -13.41835358098578723, -11.40000029085424238, -0.3335879563140091153 ) ) ;
#9943 = CARTESIAN_POINT ( 'NONE',  ( 66.41329019055577021, 5.000000000000000000, 89.50956111919107627 ) ) ;
#9944 = DIRECTION ( 'NONE',  ( -0.7071067811865451302, -0.000000000000000000, 0.7071067811865500152 ) ) ;
#9945 = CIRCLE ( 'NONE', #4754, 0.8600000000000014300 ) ;
#9946 = FACE_BOUND ( 'NONE', #873, .T. ) ;
#9947 = CARTESIAN_POINT ( 'NONE',  ( -35.58670980944424400, 2.488961461112888074, 97.50956111919106206 ) ) ;
#9948 = AXIS2_PLACEMENT_3D ( 'NONE', #4185, #11383, #5356 ) ;
#9949 = EDGE_CURVE ( 'NONE', #12943, #12948, #7571, .T. ) ;
#9950 = ORIENTED_EDGE ( 'NONE', *, *, #6520, .T. ) ;
#9951 = DIRECTION ( 'NONE',  ( 0.000000000000000000, 0.000000000000000000, -1.000000000000000000 ) ) ;
#9952 = VECTOR ( 'NONE', #3188, 1000.000000000000000 ) ;
#9953 = VERTEX_POINT ( 'NONE', #5398 ) ;
#9954 = VECTOR ( 'NONE', #3264, 1000.000000000000114 ) ;
#9955 = SURFACE_STYLE_FILL_AREA ( #14610 ) ;
#9956 = CARTESIAN_POINT ( 'NONE',  ( 3.796719365261179480, -2.062499999999996003, -1.574265350336458313 ) ) ;
#9957 = EDGE_LOOP ( 'NONE', ( #4279, #9027, #9287, #2675 ) ) ;
#9958 = CIRCLE ( 'NONE', #10449, 1.250000000000001110 ) ;
#9959 = CARTESIAN_POINT ( 'NONE',  ( 1.485839477460144442, -3.811713562373131303, 3.583429635616939724 ) ) ;
#9960 = DIRECTION ( 'NONE',  ( -1.224646799147353207E-16, -1.153910517212117582E-31, 1.000000000000000000 ) ) ;
#9961 = EDGE_CURVE ( 'NONE', #1753, #8331, #10948, .T. ) ;
#9962 = PLANE ( 'NONE',  #7815 ) ;
#9963 = AXIS2_PLACEMENT_3D ( 'NONE', #8380, #2635, #12104 ) ;
#9964 = DIRECTION ( 'NONE',  ( 1.000000000000000000, 0.000000000000000000, 0.000000000000000000 ) ) ;
#9965 = EDGE_CURVE ( 'NONE', #5280, #3825, #11123, .T. ) ;
#9966 = LINE ( 'NONE', #2842, #9628 ) ;
#9967 = DIRECTION ( 'NONE',  ( 0.000000000000000000, -0.000000000000000000, 1.000000000000000000 ) ) ;
#9968 = FACE_OUTER_BOUND ( 'NONE', #5032, .T. ) ;
#9969 = DIRECTION ( 'NONE',  ( 1.747085166004344019E-15, -1.000000000000000000, 0.000000000000000000 ) ) ;
#9970 = VECTOR ( 'NONE', #13040, 1000.000000000000000 ) ;
#9971 = CARTESIAN_POINT ( 'NONE',  ( -82.27438362643999881, 65.17411849586700612, -79.59847958357700293 ) ) ;
#9972 = ORIENTED_EDGE ( 'NONE', *, *, #1623, .F. ) ;
#9973 = ORIENTED_EDGE ( 'NONE', *, *, #14454, .F. ) ;
#9974 = CIRCLE ( 'NONE', #13939, 1.999999999999989564 ) ;
#9975 = CARTESIAN_POINT ( 'NONE',  ( -69.77438362644001302, 79.67411849586700612, -67.69567958357700377 ) ) ;
#9976 = CARTESIAN_POINT ( 'NONE',  ( -3.563362751979611165, -1.147500000000009734, 1.477520127916053694 ) ) ;
#9977 = EDGE_LOOP ( 'NONE', ( #12533, #347, #2853, #7056, #6452, #4054 ) ) ;
#9978 = AXIS2_PLACEMENT_3D ( 'NONE', #7144, #11865, #10693 ) ;
#9979 = EDGE_CURVE ( 'NONE', #455, #4992, #6256, .T. ) ;
#9980 = CIRCLE ( 'NONE', #12477, 16.00000000000000000 ) ;
#9981 = CARTESIAN_POINT ( 'NONE',  ( -1.438230851946688649, -5.195093061962212211, -3.273449327035441669 ) ) ;
#9982 = DIRECTION ( 'NONE',  ( 0.000000000000000000, 0.000000000000000000, -1.000000000000000000 ) ) ;
#9983 = ADVANCED_FACE ( 'NONE', ( #8634 ), #8870, .F. ) ;
#9984 = VECTOR ( 'NONE', #6376, 999.9999999999998863 ) ;
#9985 = DIRECTION ( 'NONE',  ( 0.000000000000000000, 0.000000000000000000, 1.000000000000000000 ) ) ;
#9986 = CARTESIAN_POINT ( 'NONE',  ( -14.25000000000000000, -0.3156864504677185379, -22.25638000318209109 ) ) ;
#9987 = CARTESIAN_POINT ( 'NONE',  ( -44.58670980944422269, 5.000000000000000000, 89.50956111919107627 ) ) ;
#9988 = EDGE_LOOP ( 'NONE', ( #1777, #1236, #9498, #3575 ) ) ;
#9989 = DIRECTION ( 'NONE',  ( -0.000000000000000000, -0.000000000000000000, -1.000000000000000000 ) ) ;
#9990 = AXIS2_PLACEMENT_3D ( 'NONE', #14587, #8397, #7555 ) ;
#9991 = CIRCLE ( 'NONE', #1081, 1.785937500000001066 ) ;
#9992 = ORIENTED_EDGE ( 'NONE', *, *, #12900, .T. ) ;
#9993 = EDGE_CURVE ( 'NONE', #8016, #9681, #3980, .T. ) ;
#9994 = ORIENTED_EDGE ( 'NONE', *, *, #7275, .T. ) ;
#9995 = VERTEX_POINT ( 'NONE', #561 ) ;
#9996 = ORIENTED_EDGE ( 'NONE', *, *, #8123, .T. ) ;
#9997 = ORIENTED_EDGE ( 'NONE', *, *, #436, .F. ) ;
#9998 = VECTOR ( 'NONE', #10349, 1000.000000000000000 ) ;
#9999 = DIRECTION ( 'NONE',  ( 8.034405899049458729E-17, 0.7547095802227716810, -0.6560590289905077199 ) ) ;
#10000 = CARTESIAN_POINT ( 'NONE',  ( -3.733522804429754149, -2.085000000000140741, 0.001371824453762974898 ) ) ;
#10001 = EDGE_CURVE ( 'NONE', #2062, #2658, #13680, .T. ) ;
#10002 = CARTESIAN_POINT ( 'NONE',  ( -2.475833455637627800, -3.640624999999937383, 3.015200003105952042 ) ) ;
#10003 = CLOSED_SHELL ( 'NONE', ( #15176, #8754, #3808, #6004, #2391, #6386, #8869 ) ) ;
#10004 = CIRCLE ( 'NONE', #4827, 3.000000000000002665 ) ;
#10005 = DIRECTION ( 'NONE',  ( -0.000000000000000000, 0.000000000000000000, -1.000000000000000000 ) ) ;
#10006 = AXIS2_PLACEMENT_3D ( 'NONE', #14405, #3791, #745 ) ;
#10007 = CARTESIAN_POINT ( 'NONE',  ( 68.41329019055577021, 5.000000000000000000, 137.5095611191910621 ) ) ;
#10008 = ADVANCED_FACE ( 'NONE', ( #6558 ), #11275, .F. ) ;
#10009 = EDGE_CURVE ( 'NONE', #8182, #7017, #7488, .T. ) ;
#10010 = CARTESIAN_POINT ( 'NONE',  ( -4.119136937081615990, 2.375954066961606159, -1.865445541641003624 ) ) ;
#10011 = CARTESIAN_POINT ( 'NONE',  ( -50.27438362644099357, 99.17411849586700612, -145.2984795835770058 ) ) ;
#10012 = LINE ( 'NONE', #13444, #11522 ) ;
#10013 = DIRECTION ( 'NONE',  ( -0.000000000000000000, 0.000000000000000000, 1.000000000000000000 ) ) ;
#10014 = B_SPLINE_CURVE_WITH_KNOTS ( 'NONE', 3,
 ( #7092, #11814, #1179, #10638 ),
 .UNSPECIFIED., .F., .F.,
 ( 4, 4 ),
 ( 0.8333333174325897597, 0.8334051513705891256 ),
 .UNSPECIFIED. ) ;
#10015 = DIRECTION ( 'NONE',  ( -1.000000000000000000, 0.000000000000000000, 0.000000000000000000 ) ) ;
#10016 = ORIENTED_EDGE ( 'NONE', *, *, #3653, .T. ) ;
#10017 = DIRECTION ( 'NONE',  ( 1.224646799147353207E-16, 1.153910517212117582E-31, 1.000000000000000000 ) ) ;
#10018 = EDGE_LOOP ( 'NONE', ( #2346, #4108, #9533 ) ) ;
#10019 = ORIENTED_EDGE ( 'NONE', *, *, #14731, .F. ) ;
#10020 = ORIENTED_EDGE ( 'NONE', *, *, #1847, .T. ) ;
#10021 = AXIS2_PLACEMENT_3D ( 'NONE', #1382, #10849, #209 ) ;
#10022 = AXIS2_PLACEMENT_3D ( 'NONE', #6276, #10838, #10909 ) ;
#10023 = CARTESIAN_POINT ( 'NONE',  ( -1.673688575075003955E-15, 4.650702586819541295, 0.000000000000000000 ) ) ;
#10024 = CARTESIAN_POINT ( 'NONE',  ( -2.968563080203957316, -6.022500000000311715, -1.228311040920463393 ) ) ;
#10025 = CARTESIAN_POINT ( 'NONE',  ( 1.375881166777175254E-16, 9.250000000000000000, 0.000000000000000000 ) ) ;
#10026 = FACE_OUTER_BOUND ( 'NONE', #517, .T. ) ;
#10027 = CARTESIAN_POINT ( 'NONE',  ( -52.77438362644000591, 65.17411849586700612, -145.4984795835769660 ) ) ;
#10028 = CARTESIAN_POINT ( 'NONE',  ( -15.50000000000000000, -0.2038245569916614930, 23.94337567297399971 ) ) ;
#10029 = CARTESIAN_POINT ( 'NONE',  ( 0.3463240970199374935, -0.4995676945082583309, 4.051387190110659731 ) ) ;
#10030 = CARTESIAN_POINT ( 'NONE',  ( 2.417253850352953481, -4.460000000000003517, 2.418486108946755309 ) ) ;
#10031 = ORIENTED_EDGE ( 'NONE', *, *, #10413, .F. ) ;
#10032 = CIRCLE ( 'NONE', #4096, 1.500000000000001332 ) ;
#10033 = DIRECTION ( 'NONE',  ( 0.8660254037844387076, 0.4999999999999998890, 0.000000000000000000 ) ) ;
#10034 = ORIENTED_EDGE ( 'NONE', *, *, #993, .F. ) ;
#10035 = DIRECTION ( 'NONE',  ( 0.8660254037844383745, -0.5000000000000003331, 0.000000000000000000 ) ) ;
#10036 = CARTESIAN_POINT ( 'NONE',  ( -2.240749814637992721, -2.656250000000047073, 3.351605112894145311 ) ) ;
#10037 = VERTEX_POINT ( 'NONE', #1582 ) ;
#10038 =( GEOMETRIC_REPRESENTATION_CONTEXT ( 3 ) GLOBAL_UNCERTAINTY_ASSIGNED_CONTEXT ( ( #11186 ) ) GLOBAL_UNIT_ASSIGNED_CONTEXT ( ( #4631, #12620, #5801 ) ) REPRESENTATION_CONTEXT ( 'NONE', 'WORKASPACE' ) );
#10039 = VECTOR ( 'NONE', #1474, 1000.000000000000000 ) ;
#10040 = DIRECTION ( 'NONE',  ( -1.000000000000000000, 0.000000000000000000, 0.000000000000000000 ) ) ;
#10041 = CARTESIAN_POINT ( 'NONE',  ( -49.02438362643999881, 65.17411849586700612, -150.4984795835770228 ) ) ;
#10042 = DIRECTION ( 'NONE',  ( 0.000000000000000000, 0.000000000000000000, -1.000000000000000000 ) ) ;
#10043 = DIRECTION ( 'NONE',  ( 0.000000000000000000, 1.000000000000000000, 0.000000000000000000 ) ) ;
#10044 = DIRECTION ( 'NONE',  ( 0.000000000000000000, 0.000000000000000000, 1.000000000000000000 ) ) ;
#10045 = CARTESIAN_POINT ( 'NONE',  ( 15.50000000000000000, -0.2000000000000000111, -19.19999999702029925 ) ) ;
#10046 = CIRCLE ( 'NONE', #4115, 8.000000000000007105 ) ;
#10047 = DIRECTION ( 'NONE',  ( 1.000000000000000000, -0.000000000000000000, -0.000000000000000000 ) ) ;
#10048 = CARTESIAN_POINT ( 'NONE',  ( -14.25000000000000000, -2.500000000000000000, -21.77831216351300014 ) ) ;
#10049 = CIRCLE ( 'NONE', #12051, 2.750000000000002665 ) ;
#10050 = VECTOR ( 'NONE', #10118, 1000.000000000000114 ) ;
#10051 = EDGE_CURVE ( 'NONE', #15273, #3516, #10097, .T. ) ;
#10052 = EDGE_LOOP ( 'NONE', ( #11116, #10905 ) ) ;
#10053 = CARTESIAN_POINT ( 'NONE',  ( -52.77438362644100067, 99.17411849586700612, -145.4984795835769944 ) ) ;
#10054 = CARTESIAN_POINT ( 'NONE',  ( -3.419120714393279137, -1.006874999999977760, -1.825951887684667208 ) ) ;
#10055 = EDGE_LOOP ( 'NONE', ( #6215, #465 ) ) ;
#10056 = ADVANCED_FACE ( 'NONE', ( #13458 ), #11047, .F. ) ;
#10057 = AXIS2_PLACEMENT_3D ( 'NONE', #6207, #14476, #3861 ) ;
#10058 = STYLED_ITEM ( 'NONE', ( #475 ), #5426 ) ;
#10059 = DIRECTION ( 'NONE',  ( 0.000000000000000000, 0.000000000000000000, 1.000000000000000000 ) ) ;
#10060 = DIRECTION ( 'NONE',  ( 0.08715574274766174634, 4.320305823558445294E-16, -0.9961946980917452121 ) ) ;
#10061 = DIRECTION ( 'NONE',  ( -9.422394424380278809E-16, 1.000000000000000000, -0.000000000000000000 ) ) ;
#10062 = FACE_OUTER_BOUND ( 'NONE', #12411, .T. ) ;
#10063 = DIRECTION ( 'NONE',  ( 0.000000000000000000, 0.000000000000000000, -1.000000000000000000 ) ) ;
#10064 = ORIENTED_EDGE ( 'NONE', *, *, #13848, .F. ) ;
#10065 = CARTESIAN_POINT ( 'NONE',  ( -38.27438362644000591, 111.1741184958670061, 0.000000000000000000 ) ) ;
#10066 = AXIS2_PLACEMENT_3D ( 'NONE', #13466, #13316, #4935 ) ;
#10067 = EDGE_CURVE ( 'NONE', #13261, #7517, #11946, .T. ) ;
#10068 = ADVANCED_FACE ( 'NONE', ( #10026 ), #9202, .F. ) ;
#10069 = ORIENTED_EDGE ( 'NONE', *, *, #11612, .T. ) ;
#10070 = AXIS2_PLACEMENT_3D ( 'NONE', #3110, #5604, #13740 ) ;
#10071 = VERTEX_POINT ( 'NONE', #495 ) ;
#10072 = ORIENTED_EDGE ( 'NONE', *, *, #13202, .T. ) ;
#10073 = ORIENTED_EDGE ( 'NONE', *, *, #3623, .F. ) ;
#10074 = ORIENTED_EDGE ( 'NONE', *, *, #11402, .F. ) ;
#10075 = CARTESIAN_POINT ( 'NONE',  ( 3.175740969752042453, -5.921088562373065578, 1.695960816590878384 ) ) ;
#10076 = AXIS2_PLACEMENT_3D ( 'NONE', #7480, #6097, #7405 ) ;
#10077 = CARTESIAN_POINT ( 'NONE',  ( 0.001419932108912198322, -3.750000000000078160, 3.886924930609184869 ) ) ;
#10078 = CARTESIAN_POINT ( 'NONE',  ( 14.24999999999999822, -0.2715193793361447838, -22.98718409945083252 ) ) ;
#10079 = CARTESIAN_POINT ( 'NONE',  ( -80.27438362643999881, 82.17411849586700612, -80.14847958357698587 ) ) ;
#10080 = EDGE_CURVE ( 'NONE', #4585, #913, #14830, .T. ) ;
#10081 = CARTESIAN_POINT ( 'NONE',  ( -3.778928804394623864, 2.374507716408091884, -2.454703312603006893 ) ) ;
#10082 = CARTESIAN_POINT ( 'NONE',  ( -3.681901511607714728, -1.578124999999909850, 1.966760930092153137 ) ) ;
#10083 = CARTESIAN_POINT ( 'NONE',  ( -52.77438362643999881, 67.53201699523744139, -150.4984795835770228 ) ) ;
#10084 = CARTESIAN_POINT ( 'NONE',  ( -50.73238362644099197, 100.3530677455522238, -147.9984795835769944 ) ) ;
#10085 = DIRECTION ( 'NONE',  ( -9.422394424380278809E-16, 1.000000000000000000, -0.000000000000000000 ) ) ;
#10086 = VERTEX_POINT ( 'NONE', #5227 ) ;
#10087 = DIRECTION ( 'NONE',  ( 0.000000000000000000, 0.000000000000000000, 1.000000000000000000 ) ) ;
#10088 = ADVANCED_FACE ( 'NONE', ( #2738, #1800 ), #640, .T. ) ;
#10089 = ORIENTED_EDGE ( 'NONE', *, *, #11679, .T. ) ;
#10090 = EDGE_LOOP ( 'NONE', ( #2289, #6908, #10122, #10831 ) ) ;
#10091 = VERTEX_POINT ( 'NONE', #12208 ) ;
#10092 = EDGE_CURVE ( 'NONE', #11817, #3095, #12291, .T. ) ;
#10093 = AXIS2_PLACEMENT_3D ( 'NONE', #1178, #2568, #14207 ) ;
#10094 = DIRECTION ( 'NONE',  ( -0.000000000000000000, 1.000000000000000000, -0.000000000000000000 ) ) ;
#10095 = EDGE_CURVE ( 'NONE', #5739, #13506, #6747, .T. ) ;
#10096 = CARTESIAN_POINT ( 'NONE',  ( -91.27438362643999881, 65.17411849586700612, -152.4984795835769944 ) ) ;
#10097 = LINE ( 'NONE', #13382, #3031 ) ;
#10098 = PLANE ( 'NONE',  #8084 ) ;
#10099 = EDGE_CURVE ( 'NONE', #1401, #9574, #1786, .T. ) ;
#10100 = CARTESIAN_POINT ( 'NONE',  ( 16.75000000000000000, -2.500000000000000000, -23.22168783648699986 ) ) ;
#10101 = CARTESIAN_POINT ( 'NONE',  ( 2.200487690058695822, -0.4995676945082536680, 3.334363425755398680 ) ) ;
#10102 =( REPRESENTATION_RELATIONSHIP ('NONE','NONE', #13541, #11263 ) REPRESENTATION_RELATIONSHIP_WITH_TRANSFORMATION ( #8880 )SHAPE_REPRESENTATION_RELATIONSHIP( ) );
#10103 = AXIS2_PLACEMENT_3D ( 'NONE', #12645, #5449, #10310 ) ;
#10104 = CYLINDRICAL_SURFACE ( 'NONE', #4241, 5.499999999999998224 ) ;
#10105 = VERTEX_POINT ( 'NONE', #15123 ) ;
#10106 = DIRECTION ( 'NONE',  ( 0.000000000000000000, -2.891205793294679017E-15, -1.000000000000000000 ) ) ;
#10107 = EDGE_CURVE ( 'NONE', #2501, #4543, #9014, .T. ) ;
#10108 = ORIENTED_EDGE ( 'NONE', *, *, #9906, .T. ) ;
#10109 = ORIENTED_EDGE ( 'NONE', *, *, #2013, .F. ) ;
#10110 = CARTESIAN_POINT ( 'NONE',  ( 1.186295216973591859, -2.203125000000055067, -3.915803815994934656 ) ) ;
#10111 = VERTEX_POINT ( 'NONE', #12597 ) ;
#10112 = AXIS2_PLACEMENT_3D ( 'NONE', #7824, #905, #15088 ) ;
#10113 = CARTESIAN_POINT ( 'NONE',  ( -52.77438362644000591, 99.17411849586700612, -152.4984795835769944 ) ) ;
#10114 = DIRECTION ( 'NONE',  ( 0.4999999999999827360, 0.000000000000000000, 0.8660254037844485886 ) ) ;
#10115 = CARTESIAN_POINT ( 'NONE',  ( 14.25000000000000000, -0.2038245569916330158, 21.77831216351300014 ) ) ;
#10116 = PLANE ( 'NONE',  #3445 ) ;
#10117 = CARTESIAN_POINT ( 'NONE',  ( 2.396990258891838366, 1.779390553524114571, 4.499999999999998224 ) ) ;
#10118 = DIRECTION ( 'NONE',  ( -0.8660254037844482555, 0.000000000000000000, -0.4999999999999831801 ) ) ;
#10119 = CARTESIAN_POINT ( 'NONE',  ( -70.92217029502012338, 98.13548005602207525, -94.57530113422089357 ) ) ;
#10120 = DIRECTION ( 'NONE',  ( 1.000000000000000000, 0.000000000000000000, 0.000000000000000000 ) ) ;
#10121 = AXIS2_PLACEMENT_3D ( 'NONE', #6726, #6658, #662 ) ;
#10122 = ORIENTED_EDGE ( 'NONE', *, *, #12106, .F. ) ;
#10123 = CARTESIAN_POINT ( 'NONE',  ( -54.81638362644100226, 97.99516924618178848, -150.4984795835770228 ) ) ;
#10124 = CARTESIAN_POINT ( 'NONE',  ( -1.487946254897667187, -0.8975000000000187272, -3.594883137563858799 ) ) ;
#10125 = ORIENTED_EDGE ( 'NONE', *, *, #14984, .T. ) ;
#10126 = CARTESIAN_POINT ( 'NONE',  ( -60.52799568714584666, 103.6741184958669919, -152.4984795835769944 ) ) ;
#10127 = CARTESIAN_POINT ( 'NONE',  ( -73.76311196519618818, 67.29799558322736175, -83.44847958357698303 ) ) ;
#10128 = CARTESIAN_POINT ( 'NONE',  ( -84.73238362644100619, 100.3530677455522238, -147.9984795835769944 ) ) ;
#10129 = FACE_OUTER_BOUND ( 'NONE', #11834, .T. ) ;
#10130 = DIRECTION ( 'NONE',  ( 1.000000000000000000, 0.000000000000000000, 0.000000000000000000 ) ) ;
#10131 = DIRECTION ( 'NONE',  ( 0.000000000000000000, 1.000000000000000000, 0.000000000000000000 ) ) ;
#10132 = EDGE_CURVE ( 'NONE', #4413, #11099, #10441, .T. ) ;
#10133 = VERTEX_POINT ( 'NONE', #3269 ) ;
#10134 = DIRECTION ( 'NONE',  ( 0.000000000000000000, 6.513401669715868659E-16, -1.000000000000000000 ) ) ;
#10135 = EDGE_LOOP ( 'NONE', ( #14857, #1738, #8247, #7139 ) ) ;
#10136 = ORIENTED_EDGE ( 'NONE', *, *, #6475, .T. ) ;
#10137 = ORIENTED_EDGE ( 'NONE', *, *, #1623, .T. ) ;
#10138 = ORIENTED_EDGE ( 'NONE', *, *, #997, .F. ) ;
#10139 = ORIENTED_EDGE ( 'NONE', *, *, #12964, .T. ) ;
#10140 = CARTESIAN_POINT ( 'NONE',  ( -2.332209567415143514, -5.358588562372849751, -2.839672270176649693 ) ) ;
#10141 = CARTESIAN_POINT ( 'NONE',  ( -3.976927128516043908, -0.1006259897310523566, 0.3906606232675376988 ) ) ;
#10142 = DIRECTION ( 'NONE',  ( 0.000000000000000000, 1.000000000000000000, 0.000000000000000000 ) ) ;
#10143 = PRODUCT_DEFINITION ( 'UNKNOWN', '', #8911, #635 ) ;
#10144 = CARTESIAN_POINT ( 'NONE',  ( 2.541707380700019225, -2.859374999999939160, 3.094782911937220771 ) ) ;
#10145 = DIRECTION ( 'NONE',  ( 0.000000000000000000, 0.000000000000000000, 1.000000000000000000 ) ) ;
#10146 = EDGE_CURVE ( 'NONE', #7767, #12014, #14975, .T. ) ;
#10147 = DIRECTION ( 'NONE',  ( -1.000000000000000000, 0.000000000000000000, 0.000000000000000000 ) ) ;
#10148 = DIRECTION ( 'NONE',  ( 0.000000000000000000, 4.336808689942017736E-16, -1.000000000000000000 ) ) ;
#10149 = CARTESIAN_POINT ( 'NONE',  ( 3.919974135967671636, -1.062500000000018652, -1.622483930095183213 ) ) ;
#10150 = CARTESIAN_POINT ( 'NONE',  ( 3.372444421885775423, -0.4995676945082423992, 2.006840812041871924 ) ) ;
#10151 = CARTESIAN_POINT ( 'NONE',  ( -89.27438362644100778, 99.17411849586700612, -79.59847958357700293 ) ) ;
#10152 = EDGE_CURVE ( 'NONE', #8835, #4666, #989, .T. ) ;
#10153 = DIRECTION ( 'NONE',  ( 0.000000000000000000, 0.000000000000000000, -1.000000000000000000 ) ) ;
#10154 = ORIENTED_EDGE ( 'NONE', *, *, #8364, .F. ) ;
#10155 = LINE ( 'NONE', #6401, #7778 ) ;
#10156 = ORIENTED_EDGE ( 'NONE', *, *, #7629, .F. ) ;
#10157 = ORIENTED_EDGE ( 'NONE', *, *, #14428, .T. ) ;
#10158 = EDGE_LOOP ( 'NONE', ( #1514, #7208, #6749, #10490, #57 ) ) ;
#10159 = CARTESIAN_POINT ( 'NONE',  ( -69.77438362644001302, 82.17411849586700612, -112.9984795835769944 ) ) ;
#10160 = DIRECTION ( 'NONE',  ( 0.000000000000000000, 0.000000000000000000, 1.000000000000000000 ) ) ;
#10161 = CARTESIAN_POINT ( 'NONE',  ( -85.75338362643999801, 63.40569462133917256, -147.9984795835769944 ) ) ;
#10162 = EDGE_CURVE ( 'NONE', #12096, #7439, #13832, .T. ) ;
#10163 = CARTESIAN_POINT ( 'NONE',  ( -3.476613658449256850, 7.159503395827455984E-16, 58.08258929006088067 ) ) ;
#10164 = AXIS2_PLACEMENT_3D ( 'NONE', #8181, #6949, #12916 ) ;
#10165 = DIRECTION ( 'NONE',  ( 0.000000000000000000, 0.000000000000000000, 1.000000000000000000 ) ) ;
#10166 = CARTESIAN_POINT ( 'NONE',  ( 2.864129664102274209, -0.4995676945082523357, 2.739103314933886590 ) ) ;
#10167 = DIRECTION ( 'NONE',  ( 1.000000000000000000, 0.000000000000000000, 0.000000000000000000 ) ) ;
#10168 = ADVANCED_FACE ( 'NONE', ( #9236 ), #11418, .F. ) ;
#10169 = CIRCLE ( 'NONE', #3495, 2.699999999999993960 ) ;
#10170 = CARTESIAN_POINT ( 'NONE',  ( 0.3227798623957477964, -5.350624999999817888, 3.285751646651179136 ) ) ;
#10171 = EDGE_CURVE ( 'NONE', #1058, #2748, #5698, .T. ) ;
#10172 = ORIENTED_EDGE ( 'NONE', *, *, #14456, .F. ) ;
#10173 = LINE ( 'NONE', #13839, #8347 ) ;
#10174 = VERTEX_POINT ( 'NONE', #864 ) ;
#10175 = FACE_OUTER_BOUND ( 'NONE', #14149, .T. ) ;
#10176 = EDGE_LOOP ( 'NONE', ( #6164, #10486, #3260, #2231 ) ) ;
#10177 = AXIS2_PLACEMENT_3D ( 'NONE', #13539, #3048, #2904 ) ;
#10178 = EDGE_CURVE ( 'NONE', #3597, #2640, #11201, .T. ) ;
#10179 = CARTESIAN_POINT ( 'NONE',  ( -2.385544021208493071, -0.6562499999999052980, 3.573005751195701407 ) ) ;
#10180 = EDGE_LOOP ( 'NONE', ( #13089, #12941, #11986, #12113, #283 ) ) ;
#10181 = CARTESIAN_POINT ( 'NONE',  ( -3.849161768156871499, -3.467963562373198805, -0.7666958849875432636 ) ) ;
#10182 = CONICAL_SURFACE ( 'NONE', #35, 7.999999999994774846, 0.7853981634258691003 ) ;
#10183 = DIRECTION ( 'NONE',  ( 0.000000000000000000, 0.000000000000000000, 1.000000000000000000 ) ) ;
#10184 = EDGE_CURVE ( 'NONE', #3401, #7307, #15203, .T. ) ;
#10185 = CYLINDRICAL_SURFACE ( 'NONE', #6847, 16.06499999999999773 ) ;
#10186 = DIRECTION ( 'NONE',  ( 1.000000000000000000, 0.000000000000000000, 0.000000000000000000 ) ) ;
#10187 = EDGE_CURVE ( 'NONE', #11015, #6676, #5263, .T. ) ;
#10188 = AXIS2_PLACEMENT_3D ( 'NONE', #14126, #11958, #9540 ) ;
#10189 = CYLINDRICAL_SURFACE ( 'NONE', #3691, 0.5999999999999998668 ) ;
#10190 = EDGE_CURVE ( 'NONE', #13165, #11131, #10701, .T. ) ;
#10191 = DIRECTION ( 'NONE',  ( 1.000000000000000000, 0.000000000000000000, 1.224646799147353454E-16 ) ) ;
#10192 = CARTESIAN_POINT ( 'NONE',  ( -56.85838362644099675, 99.17411849586700612, -147.9984795835769944 ) ) ;
#10193 = CARTESIAN_POINT ( 'NONE',  ( -72.48501812485920937, 97.94478668810718602, -93.86045013995706654 ) ) ;
#10194 = LINE ( 'NONE', #7594, #14654 ) ;
#10195 = VECTOR ( 'NONE', #14100, 1000.000000000000000 ) ;
#10196 = EDGE_LOOP ( 'NONE', ( #8933, #12299, #12902 ) ) ;
#10197 = SURFACE_STYLE_FILL_AREA ( #11607 ) ;
#10198 = CARTESIAN_POINT ( 'NONE',  ( -3.456628223078487050, -2.022499999999918252, -1.432834870345867984 ) ) ;
#10199 = ORIENTED_EDGE ( 'NONE', *, *, #12447, .F. ) ;
#10200 = AXIS2_PLACEMENT_3D ( 'NONE', #11158, #6447, #10130 ) ;
#10201 = CARTESIAN_POINT ( 'NONE',  ( -86.77438362643999881, 69.42411849586700612, -145.4984795835769944 ) ) ;
#10202 = AXIS2_PLACEMENT_3D ( 'NONE', #11810, #8237, #2340 ) ;
#10203 = CARTESIAN_POINT ( 'NONE',  ( -73.64736697264743270, 75.17411849586699191, -57.99847958357699440 ) ) ;
#10204 = CARTESIAN_POINT ( 'NONE',  ( -91.04813546431763882, 5.000000000000000000, 91.04813546431763882 ) ) ;
#10205 = CARTESIAN_POINT ( 'NONE',  ( -77.52077156573416516, 164.3482369917340122, -152.4984795835769944 ) ) ;
#10206 = LINE ( 'NONE', #3164, #14501 ) ;
#10207 = DIRECTION ( 'NONE',  ( -1.000000000000000000, 0.000000000000000000, 0.000000000000000000 ) ) ;
#10208 = VECTOR ( 'NONE', #11369, 1000.000000000000000 ) ;
#10209 = EDGE_LOOP ( 'NONE', ( #2435, #14302 ) ) ;
#10210 = LINE ( 'NONE', #9199, #1326 ) ;
#10211 = EDGE_LOOP ( 'NONE', ( #13113, #11474, #1900, #9897 ) ) ;
#10212 = ORIENTED_EDGE ( 'NONE', *, *, #10924, .F. ) ;
#10213 = CARTESIAN_POINT ( 'NONE',  ( -2.785343681203864552, -4.991249999999938680, -1.859602269982786105 ) ) ;
#10214 = ORIENTED_EDGE ( 'NONE', *, *, #7830, .F. ) ;
#10215 = ORIENTED_EDGE ( 'NONE', *, *, #11915, .T. ) ;
#10216 = CIRCLE ( 'NONE', #5284, 0.5999999999999998668 ) ;
#10217 = AXIS2_PLACEMENT_3D ( 'NONE', #3881, #5997, #13196 ) ;
#10218 = ORIENTED_EDGE ( 'NONE', *, *, #5864, .F. ) ;
#10219 = CARTESIAN_POINT ( 'NONE',  ( 2.994712326477856568, -5.905463562373213904, 2.002119754258344653 ) ) ;
#10220 = CARTESIAN_POINT ( 'NONE',  ( -3.419120714393278249, -1.006874999999977760, -1.825951887684714503 ) ) ;
#10221 = CIRCLE ( 'NONE', #3806, 3.750000000000003553 ) ;
#10222 = DIRECTION ( 'NONE',  ( 0.000000000000000000, 0.000000000000000000, 1.000000000000000000 ) ) ;
#10223 = CARTESIAN_POINT ( 'NONE',  ( -0.7834809220335302582, -2.718750000000123013, 3.946322201046845279 ) ) ;
#10224 = FACE_OUTER_BOUND ( 'NONE', #8373, .T. ) ;
#10225 = DIRECTION ( 'NONE',  ( 1.000000000000000000, 0.000000000000000000, 0.000000000000000000 ) ) ;
#10226 = DIRECTION ( 'NONE',  ( -1.000000000000000000, 0.000000000000000000, 0.000000000000000000 ) ) ;
#10227 = CARTESIAN_POINT ( 'NONE',  ( -2.385544021208493071, -0.6562499999999052980, 3.573005751195701407 ) ) ;
#10228 = DIRECTION ( 'NONE',  ( 0.8660254037844482555, 0.000000000000000000, 0.4999999999999831801 ) ) ;
#10229 = DIRECTION ( 'NONE',  ( 0.000000000000000000, 0.000000000000000000, 1.000000000000000000 ) ) ;
#10230 = VECTOR ( 'NONE', #9510, 1000.000000000000000 ) ;
#10231 = DIRECTION ( 'NONE',  ( -1.000000000000000000, 0.000000000000000000, 0.000000000000000000 ) ) ;
#10232 = VERTEX_POINT ( 'NONE', #5465 ) ;
#10233 = LINE ( 'NONE', #11265, #10734 ) ;
#10234 = VERTEX_POINT ( 'NONE', #10161 ) ;
#10235 = AXIS2_PLACEMENT_3D ( 'NONE', #4131, #3190, #3254 ) ;
#10236 = ORIENTED_EDGE ( 'NONE', *, *, #13695, .T. ) ;
#10237 = EDGE_LOOP ( 'NONE', ( #7545, #5743, #12750, #8764 ) ) ;
#10238 = EDGE_CURVE ( 'NONE', #1688, #7901, #5768, .T. ) ;
#10239 = CARTESIAN_POINT ( 'NONE',  ( -88.81638362644000040, 63.99516924618178848, -150.4984795835770228 ) ) ;
#10240 = AXIS2_PLACEMENT_3D ( 'NONE', #14130, #946, #5775 ) ;
#10241 = CARTESIAN_POINT ( 'NONE',  ( -1.336190917661197242, -3.897499999999990195, -3.228188129988408317 ) ) ;
#10242 = EDGE_CURVE ( 'NONE', #2764, #4822, #8225, .T. ) ;
#10243 = AXIS2_PLACEMENT_3D ( 'NONE', #1457, #129, #13025 ) ;
#10244 = CARTESIAN_POINT ( 'NONE',  ( -52.77438362644000591, 99.17411849586700612, -86.49847958357699440 ) ) ;
#10245 = CARTESIAN_POINT ( 'NONE',  ( -86.77438362643999881, 65.17411849586700612, -147.9984795835769944 ) ) ;
#10246 = DIRECTION ( 'NONE',  ( -1.000000000000000000, 0.000000000000000000, 0.000000000000000000 ) ) ;
#10247 =( BOUNDED_CURVE ( )  B_SPLINE_CURVE ( 3, ( #11665, #5715, #15144, #12681 ),
 .UNSPECIFIED., .F., .T. ) 
 B_SPLINE_CURVE_WITH_KNOTS ( ( 4, 4 ),
 ( 0.000000000000000000, 0.5053605102841580710 ),
 .UNSPECIFIED. ) 
 CURVE ( )  GEOMETRIC_REPRESENTATION_ITEM ( )  RATIONAL_B_SPLINE_CURVE ( ( 1.000000000000000000, 0.9788305577012359482, 0.9788305577012359482, 1.000000000000000000 ) ) 
 REPRESENTATION_ITEM ( '' )  );
#10248 = CARTESIAN_POINT ( 'NONE',  ( 12.65003830372715932, -3.992893622343521672E-16, 51.46292981703266634 ) ) ;
#10249 = CARTESIAN_POINT ( 'NONE',  ( 15.50000000000000000, 998.9628421096749662, 22.50000000000000000 ) ) ;
#10250 = DIRECTION ( 'NONE',  ( 0.000000000000000000, 0.000000000000000000, 1.000000000000000000 ) ) ;
#10251 = VERTEX_POINT ( 'NONE', #13975 ) ;
#10252 = CARTESIAN_POINT ( 'NONE',  ( 14.45313394609757296, -0.2715358723599912150, 23.33896727494797929 ) ) ;
#10253 = CIRCLE ( 'NONE', #12251, 0.8000000000000113687 ) ;
#10254 = CIRCLE ( 'NONE', #11009, 3.499999999999999556 ) ;
#10255 = VECTOR ( 'NONE', #13398, 999.9999999999998863 ) ;
#10256 = ORIENTED_EDGE ( 'NONE', *, *, #12013, .F. ) ;
#10257 = DIRECTION ( 'NONE',  ( 1.000000000000000000, 0.000000000000000000, 0.000000000000000000 ) ) ;
#10258 = EDGE_CURVE ( 'NONE', #6972, #2946, #8081, .T. ) ;
#10259 = ORIENTED_EDGE ( 'NONE', *, *, #1096, .F. ) ;
#10260 = CARTESIAN_POINT ( 'NONE',  ( -3.681901511607714728, -1.578124999999909850, 1.966760930092153137 ) ) ;
#10261 = VERTEX_POINT ( 'NONE', #10877 ) ;
#10262 = CARTESIAN_POINT ( 'NONE',  ( 3.813698945254171413, -1.936713562373129083, 1.578067310789440958 ) ) ;
#10263 = EDGE_CURVE ( 'NONE', #14030, #71, #5932, .T. ) ;
#10264 = DIRECTION ( 'NONE',  ( 0.000000000000000000, 1.000000000000000000, 0.000000000000000000 ) ) ;
#10265 = CARTESIAN_POINT ( 'NONE',  ( 57.41329019055577021, 5.000000000000001776, 133.4783111191910621 ) ) ;
#10266 = AXIS2_PLACEMENT_3D ( 'NONE', #11108, #2886, #6176 ) ;
#10267 = ADVANCED_FACE ( 'NONE', ( #14202 ), #235, .T. ) ;
#10268 = FACE_OUTER_BOUND ( 'NONE', #4295, .T. ) ;
#10269 = LINE ( 'NONE', #14999, #3882 ) ;
#10270 = FACE_OUTER_BOUND ( 'NONE', #2850, .T. ) ;
#10271 = DIRECTION ( 'NONE',  ( 1.000000000000000000, 0.000000000000000000, 0.000000000000000000 ) ) ;
#10272 = EDGE_CURVE ( 'NONE', #7322, #11599, #2416, .T. ) ;
#10273 = ORIENTED_EDGE ( 'NONE', *, *, #9487, .T. ) ;
#10274 = SURFACE_SIDE_STYLE ('',( #10197 ) ) ;
#10275 = CARTESIAN_POINT ( 'NONE',  ( 2.195116763761142842, -0.4287499999998638511, 3.287093781494352829 ) ) ;
#10276 = ORIENTED_EDGE ( 'NONE', *, *, #6056, .T. ) ;
#10277 = AXIS2_PLACEMENT_3D ( 'NONE', #747, #13796, #5505 ) ;
#10278 = EDGE_CURVE ( 'NONE', #3437, #12431, #9257, .T. ) ;
#10279 = EDGE_CURVE ( 'NONE', #9632, #1114, #1038, .T. ) ;
#10280 = CARTESIAN_POINT ( 'NONE',  ( 3.059130242547580814, -2.491250000000117204, 2.045191655759024396 ) ) ;
#10281 = DIRECTION ( 'NONE',  ( 0.000000000000000000, 0.000000000000000000, -1.000000000000000000 ) ) ;
#10282 = DIRECTION ( 'NONE',  ( -1.000000000000000000, 0.000000000000000000, 0.000000000000000000 ) ) ;
#10283 = COLOUR_RGB ( '', 0.72549020, 0.75294118, 0.79215686) ;
#10284 = DIRECTION ( 'NONE',  ( 0.000000000000000000, 1.000000000000000000, 0.000000000000000000 ) ) ;
#10285 = VECTOR ( 'NONE', #10970, 1000.000000000000000 ) ;
#10286 = EDGE_CURVE ( 'NONE', #5822, #3491, #11809, .T. ) ;
#10287 = FACE_OUTER_BOUND ( 'NONE', #7034, .T. ) ;
#10288 = CARTESIAN_POINT ( 'NONE',  ( 3.519978383818244350, -5.234011689638929710, 0.1468655065803234350 ) ) ;
#10289 = AXIS2_PLACEMENT_3D ( 'NONE', #14526, #9713, #8633 ) ;
#10290 = DIRECTION ( 'NONE',  ( 0.000000000000000000, 1.000000000000000000, 0.000000000000000000 ) ) ;
#10291 = DIRECTION ( 'NONE',  ( -0.000000000000000000, 0.000000000000000000, -1.000000000000000000 ) ) ;
#10292 = ORIENTED_EDGE ( 'NONE', *, *, #3736, .T. ) ;
#10293 = LINE ( 'NONE', #12786, #4300 ) ;
#10294 = ADVANCED_FACE ( 'NONE', ( #1413 ), #1323, .F. ) ;
#10295 = ORIENTED_EDGE ( 'NONE', *, *, #143, .F. ) ;
#10296 = ORIENTED_EDGE ( 'NONE', *, *, #10962, .F. ) ;
#10297 = CARTESIAN_POINT ( 'NONE',  ( 1.879752899984456604, -4.741249999999911147, -2.811701655874746741 ) ) ;
#10298 = ORIENTED_EDGE ( 'NONE', *, *, #15107, .T. ) ;
#10299 = AXIS2_PLACEMENT_3D ( 'NONE', #5689, #11565, #9302 ) ;
#10300 = VERTEX_POINT ( 'NONE', #9463 ) ;
#10301 = ORIENTED_EDGE ( 'NONE', *, *, #7175, .F. ) ;
#10302 = AXIS2_PLACEMENT_3D ( 'NONE', #11419, #4289, #10328 ) ;
#10303 = CARTESIAN_POINT ( 'NONE',  ( -3.028821173363755115, -5.592963562372932351, 2.025409581771773659 ) ) ;
#10304 = CIRCLE ( 'NONE', #13267, 4.000000000000004441 ) ;
#10305 = CARTESIAN_POINT ( 'NONE',  ( -1.872693635133505063, -0.2568750000000157852, 3.506634376076539716 ) ) ;
#10306 = DIRECTION ( 'NONE',  ( 2.551930889570659960E-15, -1.000000000000000000, -0.000000000000000000 ) ) ;
#10307 = CARTESIAN_POINT ( 'NONE',  ( 2.601763032574845536, -2.140624999999891198, -3.168547547573197232 ) ) ;
#10308 = DIRECTION ( 'NONE',  ( -1.000000000000000000, 0.000000000000000000, 0.000000000000000000 ) ) ;
#10309 = DIRECTION ( 'NONE',  ( 1.000000000000000000, 0.000000000000000000, 0.000000000000000000 ) ) ;
#10310 = DIRECTION ( 'NONE',  ( 1.000000000000000000, 0.000000000000000000, 0.000000000000000000 ) ) ;
#10311 = CARTESIAN_POINT ( 'NONE',  ( 3.298003658611986744, -0.8906249999999793499, 2.704611316345772121 ) ) ;
#10312 = CIRCLE ( 'NONE', #5637, 2.000000000000001776 ) ;
#10313 = CARTESIAN_POINT ( 'NONE',  ( -15.50000000000000000, -1.037157890325000054, -26.00000000000000000 ) ) ;
#10314 = CARTESIAN_POINT ( 'NONE',  ( -85.83938362643999653, 81.46011849586699327, -83.44847958357698303 ) ) ;
#10315 = LINE ( 'NONE', #5529, #4304 ) ;
#10316 = AXIS2_PLACEMENT_3D ( 'NONE', #5913, #1229, #1072 ) ;
#10317 = ORIENTED_EDGE ( 'NONE', *, *, #13673, .T. ) ;
#10318 = DIRECTION ( 'NONE',  ( -1.000000000000000000, 0.000000000000000000, -0.000000000000000000 ) ) ;
#10319 = ORIENTED_EDGE ( 'NONE', *, *, #2039, .F. ) ;
#10320 = EDGE_LOOP ( 'NONE', ( #9171, #5119, #8643, #15253 ) ) ;
#10321 = EDGE_LOOP ( 'NONE', ( #5595, #3922, #5154, #2267 ) ) ;
#10322 = CARTESIAN_POINT ( 'NONE',  ( -23.31553094873632759, 2.149910154642043551E-15, 56.34690893053225125 ) ) ;
#10323 = VECTOR ( 'NONE', #4450, 1000.000000000000000 ) ;
#10324 = AXIS2_PLACEMENT_3D ( 'NONE', #6480, #10165, #12523 ) ;
#10325 = LINE ( 'NONE', #4441, #1860 ) ;
#10326 = CARTESIAN_POINT ( 'NONE',  ( 3.469446951953614189E-15, -24.00000000000000000, 6.000000000000000000 ) ) ;
#10327 = LINE ( 'NONE', #12892, #1292 ) ;
#10328 = DIRECTION ( 'NONE',  ( 1.000000000000000000, 0.000000000000000000, 0.000000000000000000 ) ) ;
#10329 = DIRECTION ( 'NONE',  ( 0.000000000000000000, 1.000000000000000000, 0.000000000000000000 ) ) ;
#10330 = DIRECTION ( 'NONE',  ( -1.000000000000000000, 1.287488025362404182E-15, 0.000000000000000000 ) ) ;
#10331 = DIRECTION ( 'NONE',  ( 0.8660254037844387076, 0.4999999999999998890, 0.000000000000000000 ) ) ;
#10332 = ORIENTED_EDGE ( 'NONE', *, *, #859, .F. ) ;
#10333 = DIRECTION ( 'NONE',  ( 1.000000000000000000, 2.551930889570659960E-15, 0.000000000000000000 ) ) ;
#10334 = EDGE_CURVE ( 'NONE', #11511, #4176, #3772, .T. ) ;
#10335 = ORIENTED_EDGE ( 'NONE', *, *, #13014, .F. ) ;
#10336 = CONICAL_SURFACE ( 'NONE', #11587, 2.042000000000002036, 1.047197551196596965 ) ;
#10337 = ORIENTED_EDGE ( 'NONE', *, *, #11344, .T. ) ;
#10338 = LINE ( 'NONE', #7939, #3755 ) ;
#10339 = ORIENTED_EDGE ( 'NONE', *, *, #13341, .F. ) ;
#10340 = CARTESIAN_POINT ( 'NONE',  ( -4.136606882479101799, -0.4531250000000215938, -1.256032681398332906 ) ) ;
#10341 = ORIENTED_EDGE ( 'NONE', *, *, #12644, .F. ) ;
#10342 = CARTESIAN_POINT ( 'NONE',  ( -1.857982519382167963, -3.327338562373031383, -3.478237815464837901 ) ) ;
#10343 =( BOUNDED_CURVE ( )  B_SPLINE_CURVE ( 3, ( #4093, #8898, #13568, #5258 ),
 .UNSPECIFIED., .F., .T. ) 
 B_SPLINE_CURVE_WITH_KNOTS ( ( 4, 4 ),
 ( 0.000000000000000000, 0.5053605102841570718 ),
 .UNSPECIFIED. ) 
 CURVE ( )  GEOMETRIC_REPRESENTATION_ITEM ( )  RATIONAL_B_SPLINE_CURVE ( ( 1.000000000000000000, 0.9788305577012359482, 0.9788305577012359482, 1.000000000000000000 ) ) 
 REPRESENTATION_ITEM ( '' )  );
#10344 = LINE ( 'NONE', #3214, #537 ) ;
#10345 = CARTESIAN_POINT ( 'NONE',  ( -69.77438362644001302, 82.17411849586700612, -152.4984795835769944 ) ) ;
#10346 = VECTOR ( 'NONE', #13042, 1000.000000000000114 ) ;
#10347 = DIRECTION ( 'NONE',  ( 0.000000000000000000, 0.7547095802227716810, 0.6560590289905077199 ) ) ;
#10348 = EDGE_CURVE ( 'NONE', #1588, #10872, #6006, .T. ) ;
#10349 = DIRECTION ( 'NONE',  ( -0.000000000000000000, -0.000000000000000000, 1.000000000000000000 ) ) ;
#10350 = DIRECTION ( 'NONE',  ( -0.7933533402912378296, 0.6087614290087172142, 0.000000000000000000 ) ) ;
#10351 = CARTESIAN_POINT ( 'NONE',  ( 17.12895037488186389, -3.654606557864051197, 0.2687305842673423095 ) ) ;
#10352 = ORIENTED_EDGE ( 'NONE', *, *, #8113, .F. ) ;
#10353 = VECTOR ( 'NONE', #5248, 1000.000000000000000 ) ;
#10354 = CARTESIAN_POINT ( 'NONE',  ( 21.98164641901421135, -2.908542394189813650E-07, -0.3335879563140091153 ) ) ;
#10355 = CARTESIAN_POINT ( 'NONE',  ( -2.043454634528946823, -5.343749999999893419, -3.055809177479244632 ) ) ;
#10356 = ORIENTED_EDGE ( 'NONE', *, *, #14820, .F. ) ;
#10357 = CARTESIAN_POINT ( 'NONE',  ( 3.380062874710183074, -2.647499999999996856, -1.401527478686670491 ) ) ;
#10358 = CYLINDRICAL_SURFACE ( 'NONE', #10415, 4.250000000000003553 ) ;
#10359 = ADVANCED_FACE ( 'NONE', ( #3498 ), #7233, .F. ) ;
#10360 = DIRECTION ( 'NONE',  ( -0.08715574274766167695, 0.000000000000000000, 0.9961946980917453232 ) ) ;
#10361 = AXIS2_PLACEMENT_3D ( 'NONE', #8028, #6579, #14849 ) ;
#10362 = DIRECTION ( 'NONE',  ( 1.000000000000000000, 0.000000000000000000, -0.000000000000000000 ) ) ;
#10363 = CARTESIAN_POINT ( 'NONE',  ( -52.77438362644100067, 101.5320169952374414, -150.4984795835770228 ) ) ;
#10364 = EDGE_CURVE ( 'NONE', #8567, #6676, #3663, .T. ) ;
#10365 = LINE ( 'NONE', #2152, #12198 ) ;
#10366 = EDGE_CURVE ( 'NONE', #6229, #8371, #1736, .T. ) ;
#10367 = VERTEX_POINT ( 'NONE', #10011 ) ;
#10368 = LINE ( 'NONE', #10522, #9492 ) ;
#10369 = EDGE_LOOP ( 'NONE', ( #12619, #1337, #14562, #9684 ) ) ;
#10370 = ORIENTED_EDGE ( 'NONE', *, *, #4679, .T. ) ;
#10371 = CARTESIAN_POINT ( 'NONE',  ( 0.0008557816480051286256, -4.835000000000089670, -3.369777484087370656 ) ) ;
#10372 = ORIENTED_EDGE ( 'NONE', *, *, #912, .F. ) ;
#10373 = ORIENTED_EDGE ( 'NONE', *, *, #10952, .F. ) ;
#10374 = VERTEX_POINT ( 'NONE', #4270 ) ;
#10375 = CARTESIAN_POINT ( 'NONE',  ( 1.365161570743866015, -6.186713562372902153, -3.293395229433107030 ) ) ;
#10376 = EDGE_CURVE ( 'NONE', #10851, #7901, #2526, .T. ) ;
#10377 = CARTESIAN_POINT ( 'NONE',  ( 0.3809421545653356445, -0.8193749999999933031, -3.882302026224086156 ) ) ;
#10378 = CARTESIAN_POINT ( 'NONE',  ( -69.77438362644001302, 82.17411849586700612, -80.14847958357698587 ) ) ;
#10379 = CARTESIAN_POINT ( 'NONE',  ( -3.736626632189893105, -2.562500000000080824, 1.546606261444747554 ) ) ;
#10380 = CARTESIAN_POINT ( 'NONE',  ( 4.573385150445044900, -3.618985300545107364, 6.000000000000001776 ) ) ;
#10381 = EDGE_CURVE ( 'NONE', #686, #8016, #14961, .T. ) ;
#10382 = FACE_BOUND ( 'NONE', #14440, .T. ) ;
#10383 = CARTESIAN_POINT ( 'NONE',  ( 17.12895037488186389, -12.00000029085424025, 0.2687305842673423095 ) ) ;
#10384 = DIRECTION ( 'NONE',  ( 0.000000000000000000, 0.000000000000000000, 1.000000000000000000 ) ) ;
#10385 = CARTESIAN_POINT ( 'NONE',  ( -50.73238362643999722, 66.35306774555222376, -150.4984795835770228 ) ) ;
#10386 = DIRECTION ( 'NONE',  ( 0.000000000000000000, 0.000000000000000000, -1.000000000000000000 ) ) ;
#10387 = ORIENTED_EDGE ( 'NONE', *, *, #10092, .F. ) ;
#10388 = LINE ( 'NONE', #13965, #2556 ) ;
#10389 = ORIENTED_EDGE ( 'NONE', *, *, #13441, .T. ) ;
#10390 = ORIENTED_EDGE ( 'NONE', *, *, #13615, .T. ) ;
#10391 = ORIENTED_EDGE ( 'NONE', *, *, #14188, .F. ) ;
#10392 =( REPRESENTATION_RELATIONSHIP ('NONE','NONE', #12357, #14417 ) REPRESENTATION_RELATIONSHIP_WITH_TRANSFORMATION ( #12833 )SHAPE_REPRESENTATION_RELATIONSHIP( ) );
#10393 = FACE_OUTER_BOUND ( 'NONE', #4507, .T. ) ;
#10394 = CARTESIAN_POINT ( 'NONE',  ( 2.642398951855386535, -4.475625000000026610, 2.166914421091147069 ) ) ;
#10395 = CARTESIAN_POINT ( 'NONE',  ( -52.77438362644100067, 99.17411849586700612, -149.9984795835770228 ) ) ;
#10396 = DIRECTION ( 'NONE',  ( -1.000000000000000000, 0.000000000000000000, 0.000000000000000000 ) ) ;
#10397 = CARTESIAN_POINT ( 'NONE',  ( 2.396990258880748570, 1.779390553529661467, -4.500000000000000000 ) ) ;
#10398 = FACE_OUTER_BOUND ( 'NONE', #11674, .T. ) ;
#10399 = CYLINDRICAL_SURFACE ( 'NONE', #14796, 4.000000000000000000 ) ;
#10400 = CARTESIAN_POINT ( 'NONE',  ( 16.99691247867024657, 3.529302617095105621, 1.266532794505838000 ) ) ;
#10401 = DIRECTION ( 'NONE',  ( 0.4999999999999998890, -0.8660254037844387076, 0.000000000000000000 ) ) ;
#10402 = VERTEX_POINT ( 'NONE', #1715 ) ;
#10403 = DIRECTION ( 'NONE',  ( 1.000000000000000000, 0.000000000000000000, 0.000000000000000000 ) ) ;
#10404 = ORIENTED_EDGE ( 'NONE', *, *, #5714, .T. ) ;
#10405 = ORIENTED_EDGE ( 'NONE', *, *, #2994, .T. ) ;
#10406 = DIRECTION ( 'NONE',  ( -0.000000000000000000, -0.000000000000000000, -1.000000000000000000 ) ) ;
#10407 = CONTEXT_DEPENDENT_SHAPE_REPRESENTATION ( #7743, #11669 ) ;
#10408 = EDGE_LOOP ( 'NONE', ( #3739, #1169, #6228, #608 ) ) ;
#10409 = CARTESIAN_POINT ( 'NONE',  ( 3.935370341889717682, -0.9375000000000351941, 1.628420556316443557 ) ) ;
#10410 = ORIENTED_EDGE ( 'NONE', *, *, #7629, .T. ) ;
#10411 = CARTESIAN_POINT ( 'NONE',  ( 1.517146869108012996, -3.186713562373090447, -3.659994983997363782 ) ) ;
#10412 = DIRECTION ( 'NONE',  ( 0.000000000000000000, -1.000000000000000000, -0.000000000000000000 ) ) ;
#10413 = EDGE_CURVE ( 'NONE', #13125, #1380, #293, .T. ) ;
#10414 = DIRECTION ( 'NONE',  ( 0.4999999999999827360, 0.000000000000000000, 0.8660254037844485886 ) ) ;
#10415 = AXIS2_PLACEMENT_3D ( 'NONE', #1986, #7750, #12555 ) ;
#10416 = CARTESIAN_POINT ( 'NONE',  ( 3.675091696978328493, 2.375954066961625255, -2.634554458358995710 ) ) ;
#10417 = DIRECTION ( 'NONE',  ( 0.000000000000000000, 1.000000000000000000, 0.000000000000000000 ) ) ;
#10418 = VERTEX_POINT ( 'NONE', #13958 ) ;
#10419 = CARTESIAN_POINT ( 'NONE',  ( -35.58670980944424400, 2.488961461112888074, 129.5095611191910621 ) ) ;
#10420 = FACE_OUTER_BOUND ( 'NONE', #3323, .T. ) ;
#10421 = AXIS2_PLACEMENT_3D ( 'NONE', #4933, #6263, #2741 ) ;
#10422 = SHAPE_DEFINITION_REPRESENTATION ( #4099, #13541 ) ;
#10423 = EDGE_LOOP ( 'NONE', ( #6099, #11878, #5719, #14345 ) ) ;
#10424 = CIRCLE ( 'NONE', #4491, 0.6000000000000000888 ) ;
#10425 =( NAMED_UNIT ( * ) PLANE_ANGLE_UNIT ( ) SI_UNIT ( $, .RADIAN. ) );
#10426 = CARTESIAN_POINT ( 'NONE',  ( -0.3809421545647762586, -0.8506249999999871969, -3.878187885777443444 ) ) ;
#10427 = VERTEX_POINT ( 'NONE', #8300 ) ;
#10428 = EDGE_CURVE ( 'NONE', #9846, #3619, #3267, .T. ) ;
#10429 = CARTESIAN_POINT ( 'NONE',  ( -1.750120246539625946, -2.256875000000012843, 3.272202384321437840 ) ) ;
#10430 = ADVANCED_FACE ( 'NONE', ( #10457 ), #12944, .T. ) ;
#10431 = AXIS2_PLACEMENT_3D ( 'NONE', #183, #13310, #13084 ) ;
#10432 = CARTESIAN_POINT ( 'NONE',  ( 21.98164641901421135, 11.39999970914575833, -0.3335879563140091153 ) ) ;
#10433 = DIRECTION ( 'NONE',  ( 0.000000000000000000, 0.000000000000000000, 1.000000000000000000 ) ) ;
#10434 = DIRECTION ( 'NONE',  ( 0.000000000000000000, 0.000000000000000000, -1.000000000000000000 ) ) ;
#10435 =( NAMED_UNIT ( * ) SI_UNIT ( $, .STERADIAN. ) SOLID_ANGLE_UNIT ( ) );
#10436 = CARTESIAN_POINT ( 'NONE',  ( -86.77438362644100778, 99.17411849586700612, -150.4984795835770228 ) ) ;
#10437 = DIRECTION ( 'NONE',  ( 0.000000000000000000, 0.000000000000000000, -1.000000000000000000 ) ) ;
#10438 = VERTEX_POINT ( 'NONE', #8065 ) ;
#10439 = PLANE ( 'NONE',  #4551 ) ;
#10440 = ORIENTED_EDGE ( 'NONE', *, *, #14344, .T. ) ;
#10441 = CIRCLE ( 'NONE', #7499, 2.042000000000002036 ) ;
#10442 = VERTEX_POINT ( 'NONE', #9300 ) ;
#10443 = CARTESIAN_POINT ( 'NONE',  ( -1.864549691619356464, -4.928749999999819664, -2.792029179168366682 ) ) ;
#10444 = ORIENTED_EDGE ( 'NONE', *, *, #438, .T. ) ;
#10445 = VERTEX_POINT ( 'NONE', #14040 ) ;
#10446 = EDGE_CURVE ( 'NONE', #3945, #8759, #4514, .T. ) ;
#10447 = ORIENTED_EDGE ( 'NONE', *, *, #6623, .T. ) ;
#10448 = CARTESIAN_POINT ( 'NONE',  ( 2.643008371794767886, -4.874213562373096664, 2.644382268777536016 ) ) ;
#10449 = AXIS2_PLACEMENT_3D ( 'NONE', #9853, #14584, #2485 ) ;
#10450 = CARTESIAN_POINT ( 'NONE',  ( 3.280408283555247717, -0.4912499999999521139, 2.190169342145847242 ) ) ;
#10451 = EDGE_CURVE ( 'NONE', #7767, #12872, #15146, .T. ) ;
#10452 = CARTESIAN_POINT ( 'NONE',  ( -0.001059456894846966344, -2.749999999999859224, 4.019249942169077272 ) ) ;
#10453 = PLANE ( 'NONE',  #7991 ) ;
#10454 = DIRECTION ( 'NONE',  ( 0.000000000000000000, 0.000000000000000000, -1.000000000000000000 ) ) ;
#10455 = AXIS2_PLACEMENT_3D ( 'NONE', #2221, #6963, #11687 ) ;
#10456 = DIRECTION ( 'NONE',  ( -0.08715574274766162144, 0.000000000000000000, 0.9961946980917453232 ) ) ;
#10457 = FACE_OUTER_BOUND ( 'NONE', #1301, .T. ) ;
#10458 = DIRECTION ( 'NONE',  ( -0.9961946980917452121, 7.200509705930738460E-17, -0.08715574274766156593 ) ) ;
#10459 = CARTESIAN_POINT ( 'NONE',  ( -77.52077156573416516, 0.000000000000000000, -73.34256232478206528 ) ) ;
#10460 = CARTESIAN_POINT ( 'NONE',  ( -0.6461339251375918247, -5.303750000000252207, 3.244047683681893446 ) ) ;
#10461 = CARTESIAN_POINT ( 'NONE',  ( -64.53565528768383786, 67.29799558322736175, -83.44847958357698303 ) ) ;
#10462 = ADVANCED_FACE ( 'NONE', ( #12881 ), #5992, .F. ) ;
#10463 = ORIENTED_EDGE ( 'NONE', *, *, #4090, .F. ) ;
#10464 = EDGE_CURVE ( 'NONE', #6904, #3116, #2168, .T. ) ;
#10465 = DIRECTION ( 'NONE',  ( -1.000000000000000000, 0.000000000000000000, 0.000000000000000000 ) ) ;
#10466 = AXIS2_PLACEMENT_3D ( 'NONE', #578, #2397, #2923 ) ;
#10467 = ORIENTED_EDGE ( 'NONE', *, *, #15156, .F. ) ;
#10468 = ORIENTED_EDGE ( 'NONE', *, *, #1095, .F. ) ;
#10469 = ORIENTED_EDGE ( 'NONE', *, *, #1047, .T. ) ;
#10470 = EDGE_CURVE ( 'NONE', #4759, #10610, #12930, .T. ) ;
#10471 = AXIS2_PLACEMENT_3D ( 'NONE', #4600, #8243, #10565 ) ;
#10472 = FACE_OUTER_BOUND ( 'NONE', #4956, .T. ) ;
#10473 = EDGE_CURVE ( 'NONE', #10769, #8820, #12189, .T. ) ;
#10474 = DIRECTION ( 'NONE',  ( -1.287488025362404182E-15, -1.000000000000000000, 0.000000000000000000 ) ) ;
#10475 = DIRECTION ( 'NONE',  ( 0.000000000000000000, 0.000000000000000000, 1.000000000000000000 ) ) ;
#10476 = CIRCLE ( 'NONE', #3800, 2.399999999999999467 ) ;
#10477 = CARTESIAN_POINT ( 'NONE',  ( -14.25000000000000178, -0.2714405302574902090, 22.01253933645463690 ) ) ;
#10478 = VECTOR ( 'NONE', #7781, 1000.000000000000000 ) ;
#10479 = DIRECTION ( 'NONE',  ( 0.000000000000000000, -0.000000000000000000, 1.000000000000000000 ) ) ;
#10480 = DIRECTION ( 'NONE',  ( 1.000000000000000000, 0.000000000000000000, 0.000000000000000000 ) ) ;
#10481 = DIRECTION ( 'NONE',  ( 0.000000000000000000, 0.000000000000000000, 1.000000000000000000 ) ) ;
#10482 = DIRECTION ( 'NONE',  ( 0.08715574274766037244, -0.000000000000000000, -0.9961946980917454342 ) ) ;
#10483 = CARTESIAN_POINT ( 'NONE',  ( 21.98164641901421135, -12.00000029085423314, -14.73358795631400575 ) ) ;
#10484 = VERTEX_POINT ( 'NONE', #15039 ) ;
#10485 = DIRECTION ( 'NONE',  ( 0.000000000000000000, -1.000000000000000000, 0.000000000000000000 ) ) ;
#10486 = ORIENTED_EDGE ( 'NONE', *, *, #12451, .F. ) ;
#10487 = ORIENTED_EDGE ( 'NONE', *, *, #8193, .F. ) ;
#10488 = CARTESIAN_POINT ( 'NONE',  ( -77.52077156573416516, 0.000000000000000000, -79.59847958357700293 ) ) ;
#10489 = CONICAL_SURFACE ( 'NONE', #2829, 1732.050807568785558, 1.047197551196574761 ) ;
#10490 = ORIENTED_EDGE ( 'NONE', *, *, #1287, .F. ) ;
#10491 = AXIS2_PLACEMENT_3D ( 'NONE', #8431, #9432, #2618 ) ;
#10492 = EDGE_CURVE ( 'NONE', #1313, #4888, #4428, .T. ) ;
#10493 = CARTESIAN_POINT ( 'NONE',  ( 1.953452353076893244, -1.828124999999917399, 3.651470988527475647 ) ) ;
#10494 = VERTEX_POINT ( 'NONE', #3715 ) ;
#10495 = CARTESIAN_POINT ( 'NONE',  ( 2.277851013824919058, -2.155463562373088671, -3.407093304313265847 ) ) ;
#10496 = DIRECTION ( 'NONE',  ( 1.000000000000000000, 0.000000000000000000, 0.000000000000000000 ) ) ;
#10497 = FACE_BOUND ( 'NONE', #11002, .T. ) ;
#10498 = DIRECTION ( 'NONE',  ( 0.000000000000000000, 0.000000000000000000, 1.000000000000000000 ) ) ;
#10499 = CONICAL_SURFACE ( 'NONE', #93, 1732.050807568785558, 1.047197551196574761 ) ;
#10500 = AXIS2_PLACEMENT_3D ( 'NONE', #2547, #2859, #7607 ) ;
#10501 = ORIENTED_EDGE ( 'NONE', *, *, #10278, .F. ) ;
#10502 = CARTESIAN_POINT ( 'NONE',  ( 17.21626540049105003, -12.00000029085423670, -12.20299797093198535 ) ) ;
#10503 = DIRECTION ( 'NONE',  ( 0.000000000000000000, 0.000000000000000000, 1.000000000000000000 ) ) ;
#10504 = DIRECTION ( 'NONE',  ( 0.000000000000000000, 0.000000000000000000, 1.000000000000000000 ) ) ;
#10505 = ORIENTED_EDGE ( 'NONE', *, *, #12470, .F. ) ;
#10506 = CARTESIAN_POINT ( 'NONE',  ( -15.29633693294650421, -0.2717122460102743275, 21.17420925361331641 ) ) ;
#10507 = CARTESIAN_POINT ( 'NONE',  ( 3.701456747302541928, -5.015624999999988454, -0.3659357139933352987 ) ) ;
#10508 = EDGE_LOOP ( 'NONE', ( #15091, #14649, #1853, #13622 ) ) ;
#10509 = CIRCLE ( 'NONE', #845, 0.8600000000000014300 ) ;
#10510 = CIRCLE ( 'NONE', #1351, 2.514916625122320948 ) ;
#10511 = CARTESIAN_POINT ( 'NONE',  ( -2.896649075160178111, -1.975624999999826548, -2.378478989283399514 ) ) ;
#10512 = DIRECTION ( 'NONE',  ( 0.000000000000000000, -1.000000000000000000, 0.000000000000000000 ) ) ;
#10513 = DIRECTION ( 'NONE',  ( 0.000000000000000000, -1.000000000000000000, 0.000000000000000000 ) ) ;
#10514 = CARTESIAN_POINT ( 'NONE',  ( -86.77438362644001302, 65.17411849586700612, -145.4984795835769660 ) ) ;
#10515 = LINE ( 'NONE', #5811, #305 ) ;
#10516 = LINE ( 'NONE', #14099, #12284 ) ;
#10517 = ADVANCED_FACE ( 'NONE', ( #7453 ), #9673, .T. ) ;
#10518 = DIRECTION ( 'NONE',  ( -0.000000000000000000, 1.000000000000000000, 0.000000000000000000 ) ) ;
#10519 = CIRCLE ( 'NONE', #9322, 4.249999999999996447 ) ;
#10520 = EDGE_LOOP ( 'NONE', ( #12260, #4725, #15078, #6525 ) ) ;
#10521 = AXIS2_PLACEMENT_3D ( 'NONE', #13883, #7149, #12962 ) ;
#10522 = CARTESIAN_POINT ( 'NONE',  ( -15.50000000000000000, -1.037157890325000054, 22.50000000000000000 ) ) ;
#10523 = EDGE_CURVE ( 'NONE', #4906, #6230, #6287, .T. ) ;
#10524 = ORIENTED_EDGE ( 'NONE', *, *, #14094, .F. ) ;
#10525 = ORIENTED_EDGE ( 'NONE', *, *, #13317, .F. ) ;
#10526 = CARTESIAN_POINT ( 'NONE',  ( -3.450064735799972748, -4.100625000000076348, 0.3410961574374388183 ) ) ;
#10527 = EDGE_LOOP ( 'NONE', ( #2447, #9841, #8435, #6211 ) ) ;
#10528 = ORIENTED_EDGE ( 'NONE', *, *, #3225, .T. ) ;
#10529 = ORIENTED_EDGE ( 'NONE', *, *, #5742, .F. ) ;
#10530 = CARTESIAN_POINT ( 'NONE',  ( -1.409846828270459262, -5.311713562373262754, -3.400129758324495377 ) ) ;
#10531 = MANIFOLD_SOLID_BREP ( 'Cut-Extrude1[5]', #14005 ) ;
#10532 = CARTESIAN_POINT ( 'NONE',  ( -86.27438362644001302, 82.17411849586700612, -150.4984795835769944 ) ) ;
#10533 = CIRCLE ( 'NONE', #6110, 3.499999999999999556 ) ;
#10534 = AXIS2_PLACEMENT_3D ( 'NONE', #7897, #12627, #6741 ) ;
#10535 = PLANE ( 'NONE',  #2393 ) ;
#10536 = CARTESIAN_POINT ( 'NONE',  ( 10.10406781373725771, -11.00000029085428110, 69.08979243323354069 ) ) ;
#10537 = FACE_OUTER_BOUND ( 'NONE', #14867, .T. ) ;
#10538 = DIRECTION ( 'NONE',  ( 0.000000000000000000, -1.000000000000000000, 0.000000000000000000 ) ) ;
#10539 = DIRECTION ( 'NONE',  ( 1.000000000000000000, 0.000000000000000000, 0.000000000000000000 ) ) ;
#10540 = LINE ( 'NONE', #2322, #13038 ) ;
#10541 = EDGE_CURVE ( 'NONE', #14951, #1333, #2782, .T. ) ;
#10542 = FACE_OUTER_BOUND ( 'NONE', #8575, .T. ) ;
#10543 = CARTESIAN_POINT ( 'NONE',  ( -2.763334307196396722, -5.178749999999838316, 1.847896475581856324 ) ) ;
#10544 = DIRECTION ( 'NONE',  ( 0.000000000000000000, 0.000000000000000000, 1.000000000000000000 ) ) ;
#10545 = ORIENTED_EDGE ( 'NONE', *, *, #967, .F. ) ;
#10546 = CARTESIAN_POINT ( 'NONE',  ( -15.29633693294650421, -0.2717122460102769921, -23.82579074638668715 ) ) ;
#10547 = AXIS2_PLACEMENT_3D ( 'NONE', #314, #2727, #12 ) ;
#10548 = ORIENTED_EDGE ( 'NONE', *, *, #3849, .F. ) ;
#10549 = VECTOR ( 'NONE', #4065, 1000.000000000000000 ) ;
#10550 = VERTEX_POINT ( 'NONE', #13120 ) ;
#10551 = ORIENTED_EDGE ( 'NONE', *, *, #6993, .F. ) ;
#10552 = VECTOR ( 'NONE', #8964, 1000.000000000000000 ) ;
#10553 = CARTESIAN_POINT ( 'NONE',  ( -3.535952561574606801, -3.053750000000104770, -0.7042925846621640451 ) ) ;
#10554 = ADVANCED_FACE ( 'NONE', ( #378, #6154, #14407, #220, #12169, #8524 ), #14268, .F. ) ;
#10555 = DIRECTION ( 'NONE',  ( 0.000000000000000000, 0.000000000000000000, -1.000000000000000000 ) ) ;
#10556 = AXIS2_PLACEMENT_3D ( 'NONE', #6135, #10843, #8965 ) ;
#10557 = CARTESIAN_POINT ( 'NONE',  ( 2.644209610478730266, -4.874999999999846345, 2.642267524923772370 ) ) ;
#10558 = DIRECTION ( 'NONE',  ( 1.287488025362404182E-15, 1.000000000000000000, 0.000000000000000000 ) ) ;
#10559 = CARTESIAN_POINT ( 'NONE',  ( -56.85838362643999488, 65.17411849586700612, -147.9984795835769944 ) ) ;
#10560 = AXIS2_PLACEMENT_3D ( 'NONE', #7491, #2670, #12210 ) ;
#10561 = DIRECTION ( 'NONE',  ( 0.000000000000000000, 1.000000000000000000, 0.000000000000000000 ) ) ;
#10562 = CARTESIAN_POINT ( 'NONE',  ( 1.581646419014215654, -11.75147215343038987, 0.2664120436859910290 ) ) ;
#10563 = CARTESIAN_POINT ( 'NONE',  ( -69.77438362644001302, 82.17411849586700612, -81.84847958357698872 ) ) ;
#10564 = EDGE_CURVE ( 'NONE', #3511, #71, #9152, .T. ) ;
#10565 = DIRECTION ( 'NONE',  ( 1.000000000000000000, 0.000000000000000000, 0.000000000000000000 ) ) ;
#10566 = EDGE_LOOP ( 'NONE', ( #5725, #1511 ) ) ;
#10567 = CARTESIAN_POINT ( 'NONE',  ( -69.77438362644001302, 82.17411849586700612, -51.99847958357699440 ) ) ;
#10568 = ADVANCED_FACE ( 'NONE', ( #2779 ), #1620, .F. ) ;
#10569 = EDGE_LOOP ( 'NONE', ( #2948, #13909 ) ) ;
#10570 = ADVANCED_FACE ( 'NONE', ( #14715 ), #1843, .F. ) ;
#10571 = ORIENTED_EDGE ( 'NONE', *, *, #13526, .F. ) ;
#10572 = FACE_OUTER_BOUND ( 'NONE', #7674, .T. ) ;
#10573 = AXIS2_PLACEMENT_3D ( 'NONE', #738, #2927, #9112 ) ;
#10574 = AXIS2_PLACEMENT_3D ( 'NONE', #9075, #12643, #9144 ) ;
#10575 = CARTESIAN_POINT ( 'NONE',  ( -101.2743836264399988, 60.67411849586700612, -67.49847958357700861 ) ) ;
#10576 = ORIENTED_EDGE ( 'NONE', *, *, #6408, .F. ) ;
#10577 = CARTESIAN_POINT ( 'NONE',  ( 0.3887688439250656658, -3.233588562373015396, -3.936630488393996430 ) ) ;
#10578 = EDGE_CURVE ( 'NONE', #9247, #8981, #6518, .T. ) ;
#10579 = DIRECTION ( 'NONE',  ( 0.000000000000000000, -0.1240337885538713436, 0.9922779949676268085 ) ) ;
#10580 = CARTESIAN_POINT ( 'NONE',  ( -9.503456061879928640, -12.00000029085427222, 69.60114695342350899 ) ) ;
#10581 = CARTESIAN_POINT ( 'NONE',  ( -84.02438362643999881, 65.17411849586700612, -145.4984795835769944 ) ) ;
#10582 = EDGE_CURVE ( 'NONE', #6231, #10427, #11089, .T. ) ;
#10583 = AXIS2_PLACEMENT_3D ( 'NONE', #5971, #10669, #2450 ) ;
#10584 = CARTESIAN_POINT ( 'NONE',  ( -52.77438362644100067, 99.17411849586700612, -147.9984795835769944 ) ) ;
#10585 = ORIENTED_EDGE ( 'NONE', *, *, #8854, .T. ) ;
#10586 = DIRECTION ( 'NONE',  ( -0.000000000000000000, 1.000000000000000000, -0.000000000000000000 ) ) ;
#10587 = DIRECTION ( 'NONE',  ( 1.000000000000000000, 0.000000000000000000, 0.000000000000000000 ) ) ;
#10588 = MANIFOLD_SOLID_BREP ( 'Cut-Extrude4', #6072 ) ;
#10589 = SHAPE_DEFINITION_REPRESENTATION ( #2856, #12357 ) ;
#10590 = ORIENTED_EDGE ( 'NONE', *, *, #14365, .F. ) ;
#10591 = LINE ( 'NONE', #8421, #5108 ) ;
#10592 = CARTESIAN_POINT ( 'NONE',  ( -0.001042462806621457638, -0.3350000000001150946, 3.965061882346497590 ) ) ;
#10593 = ORIENTED_EDGE ( 'NONE', *, *, #13959, .F. ) ;
#10594 = VECTOR ( 'NONE', #866, 1000.000000000000000 ) ;
#10595 = CARTESIAN_POINT ( 'NONE',  ( -0.7236788045118704993, -2.303749999999964437, 3.633254187536902435 ) ) ;
#10596 = LINE ( 'NONE', #1133, #7385 ) ;
#10597 = CARTESIAN_POINT ( 'NONE',  ( 1.403561989263864891E-14, -5.500000000000007994, 0.000000000000000000 ) ) ;
#10598 = DIRECTION ( 'NONE',  ( 0.000000000000000000, 1.000000000000000000, 0.000000000000000000 ) ) ;
#10599 = CARTESIAN_POINT ( 'NONE',  ( 1.403561989263863629E-14, -5.500000000000003553, 0.000000000000000000 ) ) ;
#10600 = DIRECTION ( 'NONE',  ( -1.000000000000000000, 0.000000000000000000, 0.000000000000000000 ) ) ;
#10601 = CIRCLE ( 'NONE', #13349, 10.50000000000000178 ) ;
#10602 = ORIENTED_EDGE ( 'NONE', *, *, #1466, .F. ) ;
#10603 = CARTESIAN_POINT ( 'NONE',  ( 1.951563910473907981E-15, 7.362500000000000711, 0.000000000000000000 ) ) ;
#10604 =( NAMED_UNIT ( * ) SI_UNIT ( $, .STERADIAN. ) SOLID_ANGLE_UNIT ( ) );
#10605 = ORIENTED_EDGE ( 'NONE', *, *, #6161, .T. ) ;
#10606 = ORIENTED_EDGE ( 'NONE', *, *, #2992, .F. ) ;
#10607 = CARTESIAN_POINT ( 'NONE',  ( 3.341349309646173715, -4.553750000000432507, 0.6655201449779076794 ) ) ;
#10608 = ORIENTED_EDGE ( 'NONE', *, *, #3510, .T. ) ;
#10609 = ORIENTED_EDGE ( 'NONE', *, *, #1091, .T. ) ;
#10610 = VERTEX_POINT ( 'NONE', #14792 ) ;
#10611 = CARTESIAN_POINT ( 'NONE',  ( 1.073618264594249583, -5.202338562372997188, -3.535945309138720738 ) ) ;
#10612 = B_SPLINE_CURVE_WITH_KNOTS ( 'NONE', 3,
 ( #12690, #9349, #3384, #8116, #10506, #15235 ),
 .UNSPECIFIED., .F., .F.,
 ( 4, 2, 4 ),
 ( 0.0002380763768132926339, 0.7291065797294586925, 1.457975083082104106 ),
 .UNSPECIFIED. ) ;
#10613 = DIRECTION ( 'NONE',  ( 0.000000000000000000, 1.000000000000000000, 0.000000000000000000 ) ) ;
#10614 = VECTOR ( 'NONE', #1842, 1000.000000000000000 ) ;
#10615 = CARTESIAN_POINT ( 'NONE',  ( 10.10406781373725948, 11.99999970914572955, 69.08979243323354069 ) ) ;
#10616 = DIRECTION ( 'NONE',  ( 0.000000000000000000, 0.000000000000000000, 1.000000000000000000 ) ) ;
#10617 = ADVANCED_FACE ( 'NONE', ( #7682 ), #11236, .F. ) ;
#10618 = DIRECTION ( 'NONE',  ( -1.000000000000000000, 0.000000000000000000, 0.000000000000000000 ) ) ;
#10619 = DIRECTION ( 'NONE',  ( 0.000000000000000000, 0.000000000000000000, -1.000000000000000000 ) ) ;
#10620 = DIRECTION ( 'NONE',  ( -1.000000000000000000, -9.422394424380278809E-16, 0.000000000000000000 ) ) ;
#10621 = FACE_BOUND ( 'NONE', #12018, .T. ) ;
#10622 = CARTESIAN_POINT ( 'NONE',  ( 2.229831107420913838, -3.725624999999957776, -2.719112200499452126 ) ) ;
#10623 = DIRECTION ( 'NONE',  ( 0.000000000000000000, 1.000000000000000000, 0.000000000000000000 ) ) ;
#10624 = VERTEX_POINT ( 'NONE', #8831 ) ;
#10625 = CYLINDRICAL_SURFACE ( 'NONE', #13726, 2.500000000000002220 ) ;
#10626 = EDGE_LOOP ( 'NONE', ( #14141, #12092, #6503, #8913 ) ) ;
#10627 = ORIENTED_EDGE ( 'NONE', *, *, #3844, .F. ) ;
#10628 = ORIENTED_EDGE ( 'NONE', *, *, #6225, .T. ) ;
#10629 = EDGE_CURVE ( 'NONE', #11758, #1067, #11455, .T. ) ;
#10630 = CARTESIAN_POINT ( 'NONE',  ( 2.822884439542639790, -2.694375000000075460, -2.318423337397389261 ) ) ;
#10631 = PLANE ( 'NONE',  #2601 ) ;
#10632 = CARTESIAN_POINT ( 'NONE',  ( 3.555702576009056148, -5.046874999999973355, -1.077603027457875395 ) ) ;
#10633 = LINE ( 'NONE', #7005, #9459 ) ;
#10634 = EDGE_CURVE ( 'NONE', #11284, #4095, #10973, .T. ) ;
#10635 = FACE_OUTER_BOUND ( 'NONE', #14804, .T. ) ;
#10636 = MANIFOLD_SOLID_BREP ( 'Cut-Extrude3', #1340 ) ;
#10637 = CARTESIAN_POINT ( 'NONE',  ( -15.91434062215689060, -0.3156604612129251808, 23.70415600323552852 ) ) ;
#10638 = CARTESIAN_POINT ( 'NONE',  ( -4.296227084909979510, -0.4995677573761841406, -0.01166785054812304046 ) ) ;
#10639 = DIRECTION ( 'NONE',  ( 0.000000000000000000, 0.000000000000000000, -1.000000000000000000 ) ) ;
#10640 = CARTESIAN_POINT ( 'NONE',  ( -86.77438362643999881, 65.17411849586700612, -147.9984795835769944 ) ) ;
#10641 = CARTESIAN_POINT ( 'NONE',  ( 3.897114317029974462, 9.945166405816860437E-15, 2.249999999999999556 ) ) ;
#10642 = ORIENTED_EDGE ( 'NONE', *, *, #4515, .F. ) ;
#10643 = FACE_OUTER_BOUND ( 'NONE', #14, .T. ) ;
#10644 = ORIENTED_EDGE ( 'NONE', *, *, #1466, .T. ) ;
#10645 = ORIENTED_EDGE ( 'NONE', *, *, #14987, .F. ) ;
#10646 = DIRECTION ( 'NONE',  ( 0.9961946980917452121, -3.779777825264104572E-17, 0.08715574274766174634 ) ) ;
#10647 = CARTESIAN_POINT ( 'NONE',  ( -3.133198094827410518, 0.3749999999998852029, 3.135448188384045931 ) ) ;
#10648 = EDGE_LOOP ( 'NONE', ( #588, #6925 ) ) ;
#10649 = EDGE_CURVE ( 'NONE', #1855, #11286, #12204, .T. ) ;
#10650 = CARTESIAN_POINT ( 'NONE',  ( -4.162815442996374848, -1.514838562373068909, 0.4115216691269514837 ) ) ;
#10651 = FACE_OUTER_BOUND ( 'NONE', #3848, .T. ) ;
#10652 = EDGE_CURVE ( 'NONE', #6972, #2099, #3542, .T. ) ;
#10653 = DIRECTION ( 'NONE',  ( 1.000000000000000000, 0.000000000000000000, 0.000000000000000000 ) ) ;
#10654 = CARTESIAN_POINT ( 'NONE',  ( 15.50000000000000000, 0.000000000000000000, -22.50000000000000000 ) ) ;
#10655 = CARTESIAN_POINT ( 'NONE',  ( -50.02438362644000591, 99.17411849586700612, -152.4984795835769944 ) ) ;
#10656 = VERTEX_POINT ( 'NONE', #6821 ) ;
#10657 = CARTESIAN_POINT ( 'NONE',  ( 0.000000000000000000, 0.000000000000000000, 0.000000000000000000 ) ) ;
#10658 = DIRECTION ( 'NONE',  ( 0.000000000000000000, -1.000000000000000000, 0.000000000000000000 ) ) ;
#10659 = EDGE_CURVE ( 'NONE', #6026, #5280, #4026, .T. ) ;
#10660 = ORIENTED_EDGE ( 'NONE', *, *, #13897, .F. ) ;
#10661 =( NAMED_UNIT ( * ) PLANE_ANGLE_UNIT ( ) SI_UNIT ( $, .RADIAN. ) );
#10662 = CARTESIAN_POINT ( 'NONE',  ( -2.165165973034034685, -3.656250000000003997, 3.242962682996374912 ) ) ;
#10663 = ORIENTED_EDGE ( 'NONE', *, *, #9724, .T. ) ;
#10664 = ADVANCED_FACE ( 'NONE', ( #5900, #9358 ), #906, .F. ) ;
#10665 = DIRECTION ( 'NONE',  ( 0.000000000000000000, 1.000000000000000000, 0.000000000000000000 ) ) ;
#10666 = EDGE_CURVE ( 'NONE', #9779, #4992, #10515, .T. ) ;
#10667 = CARTESIAN_POINT ( 'NONE',  ( 0.5890844654258655666, -5.395954183479145350, 3.259439424676229713 ) ) ;
#10668 = ADVANCED_FACE ( 'NONE', ( #4641 ), #5664, .F. ) ;
#10669 = DIRECTION ( 'NONE',  ( 1.000000000000000000, -1.287488025362404182E-15, 0.000000000000000000 ) ) ;
#10670 = FACE_OUTER_BOUND ( 'NONE', #8208, .T. ) ;
#10671 = AXIS2_PLACEMENT_3D ( 'NONE', #1587, #2591, #7576 ) ;
#10672 = CARTESIAN_POINT ( 'NONE',  ( -84.73238362644100619, 99.17411849586700612, -147.9984795835769944 ) ) ;
#10673 = CARTESIAN_POINT ( 'NONE',  ( -35.58670980944424400, 0.000000000000000000, 97.50956111919106206 ) ) ;
#10674 = DIRECTION ( 'NONE',  ( 0.000000000000000000, 0.000000000000000000, -1.000000000000000000 ) ) ;
#10675 = VECTOR ( 'NONE', #11229, 1000.000000000000000 ) ;
#10676 = ORIENTED_EDGE ( 'NONE', *, *, #6608, .F. ) ;
#10677 = DIRECTION ( 'NONE',  ( 1.000000000000000000, 0.000000000000000000, -6.982962677686266711E-15 ) ) ;
#10678 = SHAPE_REPRESENTATION_RELATIONSHIP ( 'NONE' , 'NONE' ,  #14417, #2753 ) ;
#10679 = ORIENTED_EDGE ( 'NONE', *, *, #1489, .F. ) ;
#10680 = PRODUCT_DEFINITION_SHAPE ( 'NONE', 'NONE',  #15340 ) ;
#10681 = LINE ( 'NONE', #2459, #12748 ) ;
#10682 = CARTESIAN_POINT ( 'NONE',  ( 3.273328345814468410, -3.522500000000126974, 1.356842221127620096 ) ) ;
#10683 = EDGE_LOOP ( 'NONE', ( #14986, #11877 ) ) ;
#10684 = VERTEX_POINT ( 'NONE', #11541 ) ;
#10685 = ORIENTED_EDGE ( 'NONE', *, *, #13714, .F. ) ;
#10686 = VECTOR ( 'NONE', #10264, 1000.000000000000000 ) ;
#10687 = CARTESIAN_POINT ( 'NONE',  ( 2.990110678052926296, -3.889838562373120645, 2.455230007768598011 ) ) ;
#10688 = CARTESIAN_POINT ( 'NONE',  ( -46.58670980944423690, 0.000000000000000000, 91.50956111919106206 ) ) ;
#10689 = ADVANCED_BREP_SHAPE_REPRESENTATION ( '', ( #10716, #10588, #285 ), #2528 ) ;
#10690 = AXIS2_PLACEMENT_3D ( 'NONE', #13752, #712, #3123 ) ;
#10691 = CARTESIAN_POINT ( 'NONE',  ( -37.27438362644000591, 99.17411849586700612, -152.4984795835769944 ) ) ;
#10692 = VECTOR ( 'NONE', #10437, 1000.000000000000000 ) ;
#10693 = DIRECTION ( 'NONE',  ( -1.000000000000000000, 0.000000000000000000, 0.000000000000000000 ) ) ;
#10694 = DIRECTION ( 'NONE',  ( 0.000000000000000000, -0.000000000000000000, 1.000000000000000000 ) ) ;
#10695 =( REPRESENTATION_RELATIONSHIP ('NONE','NONE', #13541, #11263 ) REPRESENTATION_RELATIONSHIP_WITH_TRANSFORMATION ( #2985 )SHAPE_REPRESENTATION_RELATIONSHIP( ) );
#10696 = DIRECTION ( 'NONE',  ( -0.7071067811865525687, -0.000000000000000000, 0.7071067811865425767 ) ) ;
#10697 = CARTESIAN_POINT ( 'NONE',  ( 14.25000000000000000, -2.500000000000000000, -21.77831216351300014 ) ) ;
#10698 = CARTESIAN_POINT ( 'NONE',  ( -69.77438362644001302, 90.17411849586700612, -29.37106258560738681 ) ) ;
#10699 = CARTESIAN_POINT ( 'NONE',  ( -3.450064735799886595, -4.100625000000076348, 0.3410961574374171690 ) ) ;
#10700 = DIRECTION ( 'NONE',  ( 1.000000000000000000, 0.000000000000000000, 0.000000000000000000 ) ) ;
#10701 = CIRCLE ( 'NONE', #7970, 0.5999999999999998668 ) ;
#10702 = ORIENTED_EDGE ( 'NONE', *, *, #2512, .T. ) ;
#10703 = FACE_OUTER_BOUND ( 'NONE', #2534, .T. ) ;
#10704 = ORIENTED_EDGE ( 'NONE', *, *, #3096, .F. ) ;
#10705 = AXIS2_PLACEMENT_3D ( 'NONE', #7859, #13894, #3198 ) ;
#10706 = ORIENTED_EDGE ( 'NONE', *, *, #10009, .T. ) ;
#10707 = EDGE_LOOP ( 'NONE', ( #3992, #2429, #9973, #1105 ) ) ;
#10708 = AXIS2_PLACEMENT_3D ( 'NONE', #1272, #3688, #14231 ) ;
#10709 =( LENGTH_UNIT ( ) NAMED_UNIT ( * ) SI_UNIT ( .MILLI., .METRE. ) );
#10710 = CARTESIAN_POINT ( 'NONE',  ( -3.184718056276182097, -3.006875000000130083, -1.703323619722481475 ) ) ;
#10711 = VECTOR ( 'NONE', #3466, 1000.000000000000114 ) ;
#10712 = CARTESIAN_POINT ( 'NONE',  ( -8.108964177917338034, 5.861171052203404620E-16, 53.66203178395558382 ) ) ;
#10713 = CARTESIAN_POINT ( 'NONE',  ( 3.567009421182318896, -4.953124999999990230, 1.083052099369142818 ) ) ;
#10714 = DIRECTION ( 'NONE',  ( -9.422394424380278809E-16, 1.000000000000000000, -0.000000000000000000 ) ) ;
#10715 = CARTESIAN_POINT ( 'NONE',  ( 15.50000000000000000, -2.500000000000000000, -21.05662432702600029 ) ) ;
#10716 = MANIFOLD_SOLID_BREP ( 'Boss-Extrude6', #13256 ) ;
#10717 = CARTESIAN_POINT ( 'NONE',  ( -47.27438362644100778, 114.1741184958670061, -79.49847958357700861 ) ) ;
#10718 = CARTESIAN_POINT ( 'NONE',  ( 4.763139720814411504, 0.04639863247564436632, -0.7500000000000013323 ) ) ;
#10719 = PLANE ( 'NONE',  #10783 ) ;
#10720 = CIRCLE ( 'NONE', #9469, 16.00000000000000000 ) ;
#10721 = DIRECTION ( 'NONE',  ( 0.5000000000000003331, 0.8660254037844384856, 0.000000000000000000 ) ) ;
#10722 = FACE_OUTER_BOUND ( 'NONE', #13023, .T. ) ;
#10723 = VERTEX_POINT ( 'NONE', #14018 ) ;
#10724 = CARTESIAN_POINT ( 'NONE',  ( 17.00398511370262256, -11.48933746301553960, 0.2918493266781312379 ) ) ;
#10725 = EDGE_CURVE ( 'NONE', #12773, #8985, #559, .T. ) ;
#10726 = ORIENTED_EDGE ( 'NONE', *, *, #8600, .F. ) ;
#10727 = AXIS2_PLACEMENT_3D ( 'NONE', #2609, #1290, #11848 ) ;
#10728 = ORIENTED_EDGE ( 'NONE', *, *, #6437, .F. ) ;
#10729 = CARTESIAN_POINT ( 'NONE',  ( -9.797174393178998714E-17, 9.500000000000000000, 0.000000000000000000 ) ) ;
#10730 = EDGE_CURVE ( 'NONE', #10232, #9060, #1054, .T. ) ;
#10731 = ORIENTED_EDGE ( 'NONE', *, *, #4000, .F. ) ;
#10732 = AXIS2_PLACEMENT_3D ( 'NONE', #5791, #5957, #1037 ) ;
#10733 = CARTESIAN_POINT ( 'NONE',  ( 3.196188167093295895, -1.889838562373073350, 2.621106922562215669 ) ) ;
#10734 = VECTOR ( 'NONE', #773, 1000.000000000000000 ) ;
#10735 = CARTESIAN_POINT ( 'NONE',  ( -87.79538362644099436, 100.9425423703948326, -147.9984795835769944 ) ) ;
#10736 = FACE_OUTER_BOUND ( 'NONE', #7212, .T. ) ;
#10737 = AXIS2_PLACEMENT_3D ( 'NONE', #3821, #8547, #6399 ) ;
#10738 = LINE ( 'NONE', #15227, #14686 ) ;
#10739 = CYLINDRICAL_SURFACE ( 'NONE', #87, 8.000000000000007105 ) ;
#10740 = EDGE_LOOP ( 'NONE', ( #12396, #11609, #8337, #1338 ) ) ;
#10741 = DIRECTION ( 'NONE',  ( 0.000000000000000000, 0.000000000000000000, -1.000000000000000000 ) ) ;
#10742 = VECTOR ( 'NONE', #12983, 1000.000000000000000 ) ;
#10743 = EDGE_CURVE ( 'NONE', #10656, #1386, #11713, .T. ) ;
#10744 = AXIS2_PLACEMENT_3D ( 'NONE', #5815, #4479, #7967 ) ;
#10745 = FACE_OUTER_BOUND ( 'NONE', #3339, .T. ) ;
#10746 = APPLICATION_PROTOCOL_DEFINITION ( 'draft international standard', 'automotive_design', 1998, #2768 ) ;
#10747 = ORIENTED_EDGE ( 'NONE', *, *, #10451, .F. ) ;
#10748 = AXIS2_PLACEMENT_3D ( 'NONE', #1039, #13002, #10417 ) ;
#10749 =( LENGTH_UNIT ( ) NAMED_UNIT ( * ) SI_UNIT ( .MILLI., .METRE. ) );
#10750 = CARTESIAN_POINT ( 'NONE',  ( 3.833377307806092649, -4.015625000000129674, -0.3765428855675501119 ) ) ;
#10751 = ORIENTED_EDGE ( 'NONE', *, *, #5087, .T. ) ;
#10752 = CARTESIAN_POINT ( 'NONE',  ( -3.563362751979704868, -1.147500000000009734, 1.477520127916053472 ) ) ;
#10753 = AXIS2_PLACEMENT_3D ( 'NONE', #14873, #10854, #15334 ) ;
#10754 = CARTESIAN_POINT ( 'NONE',  ( 16.99691247867024657, -3.779330867977714892, 1.266532794505838000 ) ) ;
#10755 = CIRCLE ( 'NONE', #12001, 0.8600000000000014300 ) ;
#10756 = CARTESIAN_POINT ( 'NONE',  ( -0.2942231418407759702, -5.377451219392755277, 3.333184271469537219 ) ) ;
#10757 = ADVANCED_FACE ( 'NONE', ( #13103 ), #1370, .F. ) ;
#10758 = EDGE_CURVE ( 'NONE', #10494, #11099, #13019, .T. ) ;
#10759 = CARTESIAN_POINT ( 'NONE',  ( -89.52438362644001302, 65.17411849586700612, -86.49847958357699440 ) ) ;
#10760 = CARTESIAN_POINT ( 'NONE',  ( -48.27438362644000591, 65.17411849586700612, -79.59847958357700293 ) ) ;
#10761 = CARTESIAN_POINT ( 'NONE',  ( -55.52438362644000591, 99.17411849586700612, -152.4984795835769944 ) ) ;
#10762 = DIRECTION ( 'NONE',  ( -1.445602896647339163E-16, 1.000000000000000000, 0.000000000000000000 ) ) ;
#10763 = ADVANCED_FACE ( 'NONE', ( #2453 ), #2377, .T. ) ;
#10764 = ORIENTED_EDGE ( 'NONE', *, *, #7828, .T. ) ;
#10765 = LINE ( 'NONE', #3865, #824 ) ;
#10766 = VECTOR ( 'NONE', #14560, 1000.000000000000114 ) ;
#10767 = CIRCLE ( 'NONE', #102, 4.499999999999997335 ) ;
#10768 = AXIS2_PLACEMENT_3D ( 'NONE', #9166, #5630, #3206 ) ;
#10769 = VERTEX_POINT ( 'NONE', #9505 ) ;
#10770 = ADVANCED_FACE ( 'NONE', ( #2690, #4946, #3699, #7129, #7204 ), #9654, .T. ) ;
#10771 = DIRECTION ( 'NONE',  ( 1.000000000000000000, 0.000000000000000000, 0.000000000000000000 ) ) ;
#10772 = ADVANCED_FACE ( 'NONE', ( #14387 ), #7359, .F. ) ;
#10773 = CARTESIAN_POINT ( 'NONE',  ( 0.6849063648203621568, -3.803749999999915143, -3.438650935610224835 ) ) ;
#10774 = VERTEX_POINT ( 'NONE', #1215 ) ;
#10775 = EDGE_LOOP ( 'NONE', ( #6607, #4740, #7364, #742 ) ) ;
#10776 = ORIENTED_EDGE ( 'NONE', *, *, #14454, .T. ) ;
#10777 = EDGE_CURVE ( 'NONE', #1406, #877, #5974, .T. ) ;
#10778 = DIRECTION ( 'NONE',  ( 0.000000000000000000, 1.000000000000000000, 0.000000000000000000 ) ) ;
#10779 = DIRECTION ( 'NONE',  ( 0.000000000000000000, 1.000000000000000000, 0.000000000000000000 ) ) ;
#10780 = AXIS2_PLACEMENT_3D ( 'NONE', #14828, #12520, #7998 ) ;
#10781 = DIRECTION ( 'NONE',  ( -1.287488025362404182E-15, -1.000000000000000000, 0.000000000000000000 ) ) ;
#10782 =( NAMED_UNIT ( * ) PLANE_ANGLE_UNIT ( ) SI_UNIT ( $, .RADIAN. ) );
#10783 = AXIS2_PLACEMENT_3D ( 'NONE', #9546, #14292, #3668 ) ;
#10784 = CYLINDRICAL_SURFACE ( 'NONE', #7826, 0.5999999999999998668 ) ;
#10785 = EDGE_CURVE ( 'NONE', #8406, #7102, #10985, .T. ) ;
#10786 = CARTESIAN_POINT ( 'NONE',  ( -3.166267757014364914, -3.163124999999988862, 1.693910156975028780 ) ) ;
#10787 = CARTESIAN_POINT ( 'NONE',  ( -52.77438362644100067, 96.81621999649657084, -147.9984795835769944 ) ) ;
#10788 = ORIENTED_EDGE ( 'NONE', *, *, #6158, .T. ) ;
#10789 = CARTESIAN_POINT ( 'NONE',  ( -15.50000000000000000, -2.500000000000000000, -21.05662432702600029 ) ) ;
#10790 = ORIENTED_EDGE ( 'NONE', *, *, #698, .F. ) ;
#10791 = ORIENTED_EDGE ( 'NONE', *, *, #13526, .T. ) ;
#10792 = ORIENTED_EDGE ( 'NONE', *, *, #8500, .T. ) ;
#10793 = EDGE_LOOP ( 'NONE', ( #5150, #9784, #9808, #8019 ) ) ;
#10794 = AXIS2_PLACEMENT_3D ( 'NONE', #8501, #6048, #13015 ) ;
#10795 = LINE ( 'NONE', #15278, #7253 ) ;
#10796 = AXIS2_PLACEMENT_3D ( 'NONE', #9279, #1140, #3311 ) ;
#10797 = CARTESIAN_POINT ( 'NONE',  ( -3.166267757014364914, -3.163124999999988862, 1.693910156975028780 ) ) ;
#10798 = FACE_BOUND ( 'NONE', #12835, .T. ) ;
#10799 = DIRECTION ( 'NONE',  ( 0.000000000000000000, 1.000000000000000000, 0.000000000000000000 ) ) ;
#10800 = DIRECTION ( 'NONE',  ( -1.000000000000000000, 0.000000000000000000, 0.000000000000000000 ) ) ;
#10801 = CARTESIAN_POINT ( 'NONE',  ( 1.634139617129772404, -12.00000029085424025, -0.3335879563140197179 ) ) ;
#10802 = CARTESIAN_POINT ( 'NONE',  ( -16.54686605390243059, -0.2715358723599923807, 23.33896727494797929 ) ) ;
#10803 = DIRECTION ( 'NONE',  ( 0.000000000000000000, 1.000000000000000000, 0.000000000000000000 ) ) ;
#10804 = CIRCLE ( 'NONE', #10547, 3.499999999999999556 ) ;
#10805 = DIRECTION ( 'NONE',  ( 0.000000000000000000, 1.000000000000000000, 0.000000000000000000 ) ) ;
#10806 = CARTESIAN_POINT ( 'NONE',  ( 57.41329019055577021, 5.000000000000001776, 129.5095611191910621 ) ) ;
#10807 = CARTESIAN_POINT ( 'NONE',  ( -1.006616814747114486E-29, -2.568816543514388222E-44, -4.500000000000000888 ) ) ;
#10808 = VERTEX_POINT ( 'NONE', #10911 ) ;
#10809 = AXIS2_PLACEMENT_3D ( 'NONE', #6279, #9655, #10762 ) ;
#10810 = CARTESIAN_POINT ( 'NONE',  ( 17.18164641901421419, -12.00000029085424380, 0.8664120436859873431 ) ) ;
#10811 = ORIENTED_EDGE ( 'NONE', *, *, #8652, .T. ) ;
#10812 = VERTEX_POINT ( 'NONE', #270 ) ;
#10813 = CARTESIAN_POINT ( 'NONE',  ( -15.50000000000000000, -0.4000000000000000222, -22.50000000000000000 ) ) ;
#10814 = CARTESIAN_POINT ( 'NONE',  ( -0.8493553515888951910, -0.2812499999999675260, -4.261981763090987307 ) ) ;
#10815 = ORIENTED_EDGE ( 'NONE', *, *, #13810, .T. ) ;
#10816 = AXIS2_PLACEMENT_3D ( 'NONE', #10459, #9221, #6918 ) ;
#10817 = CARTESIAN_POINT ( 'NONE',  ( 0.4121457528842378815, -1.233588562373086672, -4.200139271419963904 ) ) ;
#10818 = VECTOR ( 'NONE', #7715, 1000.000000000000000 ) ;
#10819 = DIRECTION ( 'NONE',  ( 0.000000000000000000, 0.000000000000000000, -1.000000000000000000 ) ) ;
#10820 = LINE ( 'NONE', #184, #2630 ) ;
#10821 = FACE_OUTER_BOUND ( 'NONE', #6491, .T. ) ;
#10822 = EDGE_CURVE ( 'NONE', #13729, #10610, #5021, .T. ) ;
#10823 = DIRECTION ( 'NONE',  ( -0.000000000000000000, -4.336808689942017736E-16, 1.000000000000000000 ) ) ;
#10824 = ORIENTED_EDGE ( 'NONE', *, *, #9712, .T. ) ;
#10825 = VECTOR ( 'NONE', #2362, 1000.000000000000000 ) ;
#10826 = FACE_OUTER_BOUND ( 'NONE', #14801, .T. ) ;
#10827 = CARTESIAN_POINT ( 'NONE',  ( 16.21690705545749367, 11.99999970914575798, 0.2773483677299301564 ) ) ;
#10828 = AXIS2_PLACEMENT_3D ( 'NONE', #1231, #2467, #2238 ) ;
#10829 = ORIENTED_EDGE ( 'NONE', *, *, #8199, .T. ) ;
#10830 = CARTESIAN_POINT ( 'NONE',  ( -0.3756913567350075311, -4.265625000000119904, -3.800190021185207545 ) ) ;
#10831 = ORIENTED_EDGE ( 'NONE', *, *, #9949, .F. ) ;
#10832 = VECTOR ( 'NONE', #11818, 1000.000000000000000 ) ;
#10833 = PRODUCT_RELATED_PRODUCT_CATEGORY ( 'part', '', ( #5218 ) ) ;
#10834 = CARTESIAN_POINT ( 'NONE',  ( 2.123627735229571822, -1.428750000000023501, 3.175715285003293253 ) ) ;
#10835 = ADVANCED_FACE ( 'NONE', ( #122 ), #4876, .F. ) ;
#10836 = DIRECTION ( 'NONE',  ( 0.000000000000000000, 1.000000000000000000, 0.000000000000000000 ) ) ;
#10837 = AXIS2_PLACEMENT_3D ( 'NONE', #7045, #4787, #9355 ) ;
#10838 = DIRECTION ( 'NONE',  ( 1.000000000000000000, 0.000000000000000000, 0.000000000000000000 ) ) ;
#10839 = EDGE_CURVE ( 'NONE', #3573, #14050, #1307, .T. ) ;
#10840 = DIRECTION ( 'NONE',  ( 0.08715574274766176022, 4.320305823558445788E-16, -0.9961946980917453232 ) ) ;
#10841 = CARTESIAN_POINT ( 'NONE',  ( -86.77438362643999881, 67.53201699523744139, -147.9984795835769944 ) ) ;
#10842 = FACE_OUTER_BOUND ( 'NONE', #5704, .T. ) ;
#10843 = DIRECTION ( 'NONE',  ( 0.000000000000000000, 0.000000000000000000, 1.000000000000000000 ) ) ;
#10844 = DIRECTION ( 'NONE',  ( 0.000000000000000000, 0.000000000000000000, 1.000000000000000000 ) ) ;
#10845 = ORIENTED_EDGE ( 'NONE', *, *, #14794, .F. ) ;
#10846 = CARTESIAN_POINT ( 'NONE',  ( -42.77438362644000591, 59.67411849586700612, -15.85886927678779834 ) ) ;
#10847 = EDGE_LOOP ( 'NONE', ( #3525, #13279, #1424, #13343 ) ) ;
#10848 = TOROIDAL_SURFACE ( 'NONE', #4164, 2.093999815491831562, 0.2500000000000000000 ) ;
#10849 = DIRECTION ( 'NONE',  ( 0.000000000000000000, 0.000000000000000000, -1.000000000000000000 ) ) ;
#10850 = CARTESIAN_POINT ( 'NONE',  ( 3.380062874710183518, -2.647499999999996856, -1.401527478686715344 ) ) ;
#10851 = VERTEX_POINT ( 'NONE', #13331 ) ;
#10852 = ORIENTED_EDGE ( 'NONE', *, *, #8103, .T. ) ;
#10853 = ORIENTED_EDGE ( 'NONE', *, *, #1919, .F. ) ;
#10854 = DIRECTION ( 'NONE',  ( -9.422394424380278809E-16, 1.000000000000000000, -0.000000000000000000 ) ) ;
#10855 = EDGE_CURVE ( 'NONE', #1795, #3176, #583, .T. ) ;
#10856 = DIRECTION ( 'NONE',  ( 0.000000000000000000, 0.000000000000000000, -1.000000000000000000 ) ) ;
#10857 = CARTESIAN_POINT ( 'NONE',  ( -56.85838362643999488, 65.17411849586700612, -147.9984795835769944 ) ) ;
#10858 = EDGE_CURVE ( 'NONE', #12262, #11654, #5331, .T. ) ;
#10859 = AXIS2_PLACEMENT_3D ( 'NONE', #6069, #9672, #10781 ) ;
#10860 = ADVANCED_FACE ( 'NONE', ( #736 ), #5249, .F. ) ;
#10861 = CARTESIAN_POINT ( 'NONE',  ( -2.598076211353315568, 0.1227504548087345604, 4.500000000000000888 ) ) ;
#10862 =( LENGTH_UNIT ( ) NAMED_UNIT ( * ) SI_UNIT ( .MILLI., .METRE. ) );
#10863 = CARTESIAN_POINT ( 'NONE',  ( -12.81835358098578403, -12.00000029085423670, -11.73358795631400930 ) ) ;
#10864 = CARTESIAN_POINT ( 'NONE',  ( 3.463329978863818770, -3.616249999999970210, -0.6879750677194342856 ) ) ;
#10865 = FACE_OUTER_BOUND ( 'NONE', #8738, .T. ) ;
#10866 = ORIENTED_EDGE ( 'NONE', *, *, #11290, .T. ) ;
#10867 = CARTESIAN_POINT ( 'NONE',  ( -84.73238362644100619, 97.99516924618178848, -147.9984795835769944 ) ) ;
#10868 = VERTEX_POINT ( 'NONE', #6659 ) ;
#10869 = EDGE_CURVE ( 'NONE', #5205, #13967, #4293, .T. ) ;
#10870 = ORIENTED_EDGE ( 'NONE', *, *, #5326, .T. ) ;
#10871 = ORIENTED_EDGE ( 'NONE', *, *, #4951, .T. ) ;
#10872 = VERTEX_POINT ( 'NONE', #6358 ) ;
#10873 = AXIS2_PLACEMENT_3D ( 'NONE', #4405, #11309, #15162 ) ;
#10874 = CYLINDRICAL_SURFACE ( 'NONE', #787, 4.000000000000004441 ) ;
#10875 = EDGE_CURVE ( 'NONE', #6249, #1167, #8739, .T. ) ;
#10876 = CARTESIAN_POINT ( 'NONE',  ( 0.000000000000000000, 0.000000000000000000, 0.000000000000000000 ) ) ;
#10877 = CARTESIAN_POINT ( 'NONE',  ( -15.50000000000000000, -2.500000000000000000, -21.05662432702600029 ) ) ;
#10878 = CARTESIAN_POINT ( 'NONE',  ( 22.58164641901421632, 11.99999970914576330, -11.73358795631400397 ) ) ;
#10879 = DIRECTION ( 'NONE',  ( 0.000000000000000000, 0.000000000000000000, -1.000000000000000000 ) ) ;
#10880 = ADVANCED_FACE ( 'NONE', ( #14923 ), #13218, .F. ) ;
#10881 = EDGE_CURVE ( 'NONE', #11082, #13238, #11465, .T. ) ;
#10882 = CARTESIAN_POINT ( 'NONE',  ( -15.70366306705060033, -0.2717122460100995229, 23.82579074638835692 ) ) ;
#10883 = DIRECTION ( 'NONE',  ( 0.000000000000000000, 1.000000000000000000, 0.000000000000000000 ) ) ;
#10884 = CARTESIAN_POINT ( 'NONE',  ( 17.21739630941073429, 3.678509596725633823, 0.07286771090926232042 ) ) ;
#10885 = CARTESIAN_POINT ( 'NONE',  ( 5.196152422706624918, 2.375000000000013323, -1.265134450516282343E-15 ) ) ;
#10886 = CARTESIAN_POINT ( 'NONE',  ( -68.42626121176255083, 89.17411849586700612, -44.11946707556887759 ) ) ;
#10887 = AXIS2_PLACEMENT_3D ( 'NONE', #7669, #13250, #5181 ) ;
#10888 = EDGE_LOOP ( 'NONE', ( #2118, #8352 ) ) ;
#10889 = LINE ( 'NONE', #2730, #427 ) ;
#10890 = ORIENTED_EDGE ( 'NONE', *, *, #12853, .T. ) ;
#10891 = ORIENTED_EDGE ( 'NONE', *, *, #7362, .T. ) ;
#10892 = FACE_OUTER_BOUND ( 'NONE', #9516, .T. ) ;
#10893 = CARTESIAN_POINT ( 'NONE',  ( 1.666359390640659743, -0.1874999999999558131, -4.027044093784315493 ) ) ;
#10894 = CARTESIAN_POINT ( 'NONE',  ( 3.296805766952802141, -0.8898385623730955540, 2.707089161679790745 ) ) ;
#10895 = CARTESIAN_POINT ( 'NONE',  ( -86.77438362644100778, 101.5320169952374414, -147.9984795835769944 ) ) ;
#10896 = CARTESIAN_POINT ( 'NONE',  ( 15.50000000000000000, -1.037157890325000054, -22.50000000000000000 ) ) ;
#10897 = DIRECTION ( 'NONE',  ( 0.000000000000000000, 1.000000000000000000, 0.000000000000000000 ) ) ;
#10898 = DIRECTION ( 'NONE',  ( 1.000000000000000000, 1.067522139062645347E-15, 0.000000000000000000 ) ) ;
#10899 = CARTESIAN_POINT ( 'NONE',  ( 4.500000000000000888, 1.148368900306797199E-14, 0.000000000000000000 ) ) ;
#10900 = ORIENTED_EDGE ( 'NONE', *, *, #2320, .F. ) ;
#10901 = DIRECTION ( 'NONE',  ( 0.000000000000000000, 0.000000000000000000, -1.000000000000000000 ) ) ;
#10902 = ORIENTED_EDGE ( 'NONE', *, *, #4198, .T. ) ;
#10903 = FILL_AREA_STYLE ('',( #6197 ) ) ;
#10904 = CARTESIAN_POINT ( 'NONE',  ( 0.7448305450414310913, -4.218749999999887201, -3.751694669322447329 ) ) ;
#10905 = ORIENTED_EDGE ( 'NONE', *, *, #4389, .T. ) ;
#10906 = APPLICATION_CONTEXT ( 'automotive_design' ) ;
#10907 = CARTESIAN_POINT ( 'NONE',  ( -52.77438362643999881, 65.17411849586700612, -146.8195303338917768 ) ) ;
#10908 = DIRECTION ( 'NONE',  ( -1.000000000000000000, 0.000000000000000000, 0.000000000000000000 ) ) ;
#10909 = DIRECTION ( 'NONE',  ( 0.000000000000000000, -0.000000000000000000, -1.000000000000000000 ) ) ;
#10910 = DIRECTION ( 'NONE',  ( 0.000000000000000000, 1.000000000000000000, 0.000000000000000000 ) ) ;
#10911 = CARTESIAN_POINT ( 'NONE',  ( -77.52077156573416516, 110.1741184958670061, -79.59847958357700293 ) ) ;
#10912 = LINE ( 'NONE', #13479, #7108 ) ;
#10913 = DIRECTION ( 'NONE',  ( 1.000000000000000000, 0.000000000000000000, 0.000000000000000000 ) ) ;
#10914 = DIRECTION ( 'NONE',  ( 0.08715574274766176022, 0.000000000000000000, -0.9961946980917453232 ) ) ;
#10915 = ORIENTED_EDGE ( 'NONE', *, *, #5650, .F. ) ;
#10916 = PLANE ( 'NONE',  #10243 ) ;
#10917 = EDGE_CURVE ( 'NONE', #2062, #13986, #13710, .T. ) ;
#10918 =( LENGTH_UNIT ( ) NAMED_UNIT ( * ) SI_UNIT ( .MILLI., .METRE. ) );
#10919 = ORIENTED_EDGE ( 'NONE', *, *, #1435, .F. ) ;
#10920 = DIRECTION ( 'NONE',  ( 2.551930889570659960E-15, -1.000000000000000000, -0.000000000000000000 ) ) ;
#10921 = CARTESIAN_POINT ( 'NONE',  ( 3.515159614179530490, -2.538124999999942677, 1.067305873498054059 ) ) ;
#10922 = ORIENTED_EDGE ( 'NONE', *, *, #3917, .T. ) ;
#10923 = ORIENTED_EDGE ( 'NONE', *, *, #5753, .F. ) ;
#10924 = EDGE_CURVE ( 'NONE', #10037, #6718, #3053, .T. ) ;
#10925 = ORIENTED_EDGE ( 'NONE', *, *, #12195, .F. ) ;
#10926 = CIRCLE ( 'NONE', #758, 4.000000000000004441 ) ;
#10927 = CARTESIAN_POINT ( 'NONE',  ( -15.50000000000000000, -0.2000000000000000111, -22.50000000000000000 ) ) ;
#10928 = CYLINDRICAL_SURFACE ( 'NONE', #10500, 1.250000000000001110 ) ;
#10929 = CIRCLE ( 'NONE', #9671, 1.449999999999999956 ) ;
#10930 = CARTESIAN_POINT ( 'NONE',  ( -2.894171431151455032, -0.4995676945082664355, -3.078752850849113099 ) ) ;
#10931 = SPHERICAL_SURFACE ( 'NONE', #15238, 0.6000000000000000888 ) ;
#10932 = CARTESIAN_POINT ( 'NONE',  ( -102.2743836264399988, 65.17411849586700612, -79.59847958357700293 ) ) ;
#10933 = ORIENTED_EDGE ( 'NONE', *, *, #15200, .F. ) ;
#10934 = CARTESIAN_POINT ( 'NONE',  ( -85.83938362643999653, 81.46011849586699327, -83.44847958357698303 ) ) ;
#10935 = ADVANCED_FACE ( 'NONE', ( #14850 ), #11222, .F. ) ;
#10936 = ORIENTED_EDGE ( 'NONE', *, *, #13673, .F. ) ;
#10937 = CIRCLE ( 'NONE', #13425, 4.000000000000004441 ) ;
#10938 = EDGE_LOOP ( 'NONE', ( #13785, #9440 ) ) ;
#10939 = ORIENTED_EDGE ( 'NONE', *, *, #7417, .T. ) ;
#10940 = ORIENTED_EDGE ( 'NONE', *, *, #2791, .F. ) ;
#10941 = ADVANCED_FACE ( 'NONE', ( #4003, #7513 ), #1605, .T. ) ;
#10942 = CARTESIAN_POINT ( 'NONE',  ( 21.98164641901421135, -12.00000029085424025, -8.183940086454239093 ) ) ;
#10943 = CARTESIAN_POINT ( 'NONE',  ( 0.0009802357451226765411, -1.834999999999918474, -3.766633749593359060 ) ) ;
#10944 = DIRECTION ( 'NONE',  ( 0.000000000000000000, 0.000000000000000000, -1.000000000000000000 ) ) ;
#10945 = CARTESIAN_POINT ( 'NONE',  ( -3.138285373062238648, -4.593749999999839240, 2.098600886432549828 ) ) ;
#10946 = DIRECTION ( 'NONE',  ( 0.9833652781161342782, 0.000000000000000000, 0.1816390095645149805 ) ) ;
#10947 = DIRECTION ( 'NONE',  ( -9.422394424380278809E-16, 1.000000000000000000, -0.000000000000000000 ) ) ;
#10948 = CIRCLE ( 'NONE', #4247, 1.500000000000001332 ) ;
#10949 = EDGE_CURVE ( 'NONE', #5814, #8154, #11141, .T. ) ;
#10950 = DIRECTION ( 'NONE',  ( -0.000000000000000000, 0.000000000000000000, -1.000000000000000000 ) ) ;
#10951 = LINE ( 'NONE', #5062, #846 ) ;
#10952 = EDGE_CURVE ( 'NONE', #13871, #8497, #11214, .T. ) ;
#10953 = CARTESIAN_POINT ( 'NONE',  ( 33.35543536254877495, -3.618985300545106920, 0.000000000000000000 ) ) ;
#10954 = CARTESIAN_POINT ( 'NONE',  ( -54.81638362644000040, 66.35306774555222376, -150.4984795835770228 ) ) ;
#10955 = CARTESIAN_POINT ( 'NONE',  ( -69.77438362644001302, 82.17411849586700612, -80.14847958357698587 ) ) ;
#10956 = ORIENTED_EDGE ( 'NONE', *, *, #7082, .T. ) ;
#10957 = DIRECTION ( 'NONE',  ( 1.287488025362404182E-15, 1.000000000000000000, 0.000000000000000000 ) ) ;
#10958 = AXIS2_PLACEMENT_3D ( 'NONE', #1374, #1454, #10914 ) ;
#10959 = EDGE_CURVE ( 'NONE', #5763, #8567, #5076, .T. ) ;
#10960 = ORIENTED_EDGE ( 'NONE', *, *, #12162, .F. ) ;
#10961 = EDGE_LOOP ( 'NONE', ( #5497, #8176, #15252, #2895 ) ) ;
#10962 = EDGE_CURVE ( 'NONE', #11302, #8597, #9974, .T. ) ;
#10963 = VECTOR ( 'NONE', #15282, 1000.000000000000114 ) ;
#10964 = DIRECTION ( 'NONE',  ( -1.747085166004344019E-15, 1.000000000000000000, -0.000000000000000000 ) ) ;
#10965 = EDGE_CURVE ( 'NONE', #2847, #6145, #3505, .T. ) ;
#10966 = CARTESIAN_POINT ( 'NONE',  ( -0.8236255389490674261, -1.280463562373061359, -4.132840929750037695 ) ) ;
#10967 = DIRECTION ( 'NONE',  ( 0.000000000000000000, -0.000000000000000000, 1.000000000000000000 ) ) ;
#10968 = DIRECTION ( 'NONE',  ( -1.000000000000000000, 0.000000000000000000, 0.000000000000000000 ) ) ;
#10969 = VECTOR ( 'NONE', #13365, 1000.000000000000000 ) ;
#10970 = DIRECTION ( 'NONE',  ( -1.000000000000000000, 0.000000000000000000, 0.000000000000000000 ) ) ;
#10971 = DIRECTION ( 'NONE',  ( -0.8660254037844381525, 0.000000000000000000, -0.5000000000000007772 ) ) ;
#10972 = LINE ( 'NONE', #2907, #11988 ) ;
#10973 = CIRCLE ( 'NONE', #1048, 10.50000000000000178 ) ;
#10974 = DIRECTION ( 'NONE',  ( 1.000000000000000000, 0.000000000000000000, -0.000000000000000000 ) ) ;
#10975 = ORIENTED_EDGE ( 'NONE', *, *, #10067, .F. ) ;
#10976 = CARTESIAN_POINT ( 'NONE',  ( -66.03636180653452925, 65.59017466835990717, -81.84847958357697451 ) ) ;
#10977 = EDGE_CURVE ( 'NONE', #10684, #11895, #2262, .T. ) ;
#10978 = AXIS2_PLACEMENT_3D ( 'NONE', #5603, #3329, #11788 ) ;
#10979 = ORIENTED_EDGE ( 'NONE', *, *, #1489, .T. ) ;
#10980 = CIRCLE ( 'NONE', #4288, 2.500000000000002220 ) ;
#10981 = SURFACE_SIDE_STYLE ('',( #9955 ) ) ;
#10982 = CARTESIAN_POINT ( 'NONE',  ( 0.0009972298945177876170, -4.250000000000088818, -3.820821809411817149 ) ) ;
#10983 = VERTEX_POINT ( 'NONE', #5859 ) ;
#10984 = CARTESIAN_POINT ( 'NONE',  ( 0.7308567215121246630, -4.780463562373078013, 3.679264497522872102 ) ) ;
#10985 = CIRCLE ( 'NONE', #8992, 4.500000000000000888 ) ;
#10986 = CARTESIAN_POINT ( 'NONE',  ( 3.783562653031121936, -1.569374999999871845, 0.3712484392075319217 ) ) ;
#10987 = CARTESIAN_POINT ( 'NONE',  ( -69.77438362644001302, 74.17411849586699191, -112.9984795835769944 ) ) ;
#10988 = AXIS2_PLACEMENT_3D ( 'NONE', #4068, #2588, #10898 ) ;
#10989 = CARTESIAN_POINT ( 'NONE',  ( -22.61828500675503761, 1.660051434983101380E-15, 48.37735134579827445 ) ) ;
#10990 = CARTESIAN_POINT ( 'NONE',  ( 57.41329019055577021, 5.000000000000001776, 93.54081111919107627 ) ) ;
#10991 = LINE ( 'NONE', #2760, #9312 ) ;
#10992 = CARTESIAN_POINT ( 'NONE',  ( -59.02799568714584666, 110.1741184958670061, -152.4984795835769944 ) ) ;
#10993 = FACE_OUTER_BOUND ( 'NONE', #471, .T. ) ;
#10994 = AXIS2_PLACEMENT_3D ( 'NONE', #11336, #1947, #10231 ) ;
#10995 = ORIENTED_EDGE ( 'NONE', *, *, #10582, .T. ) ;
#10996 = ORIENTED_EDGE ( 'NONE', *, *, #1948, .F. ) ;
#10997 =( NAMED_UNIT ( * ) PLANE_ANGLE_UNIT ( ) SI_UNIT ( $, .RADIAN. ) );
#10998 = VERTEX_POINT ( 'NONE', #6934 ) ;
#10999 = CARTESIAN_POINT ( 'NONE',  ( -1.629699455448989389E-14, 8.699999999999999289, 5.655858585055787181E-29 ) ) ;
#11000 = CARTESIAN_POINT ( 'NONE',  ( -2.557519727433407386, -2.960000000000007958, -2.558839988362046292 ) ) ;
#11001 = EDGE_LOOP ( 'NONE', ( #11624, #13761, #1276, #9531 ) ) ;
#11002 = EDGE_LOOP ( 'NONE', ( #4374, #12035 ) ) ;
#11003 = VECTOR ( 'NONE', #338, 1000.000000000000000 ) ;
#11004 = AXIS2_PLACEMENT_3D ( 'NONE', #1213, #3463, #5972 ) ;
#11005 = DIRECTION ( 'NONE',  ( 0.000000000000000000, 0.000000000000000000, -1.000000000000000000 ) ) ;
#11006 = DIRECTION ( 'NONE',  ( 0.000000000000000000, -1.000000000000000000, 0.000000000000000000 ) ) ;
#11007 = CARTESIAN_POINT ( 'NONE',  ( 15.50000000000000000, -5.000000000000000000, 18.50000000000000000 ) ) ;
#11008 = PLANE ( 'NONE',  #8131 ) ;
#11009 = AXIS2_PLACEMENT_3D ( 'NONE', #7463, #14581, #4037 ) ;
#11010 = EDGE_CURVE ( 'NONE', #263, #14022, #7521, .T. ) ;
#11011 = AXIS2_PLACEMENT_3D ( 'NONE', #6093, #10805, #3504 ) ;
#11012 = CARTESIAN_POINT ( 'NONE',  ( 4.573385150445044900, -3.618985300545107364, 0.000000000000000000 ) ) ;
#11013 = ORIENTED_EDGE ( 'NONE', *, *, #430, .F. ) ;
#11014 = DIRECTION ( 'NONE',  ( 0.000000000000000000, 0.000000000000000000, -1.000000000000000000 ) ) ;
#11015 = VERTEX_POINT ( 'NONE', #10641 ) ;
#11016 = VERTEX_POINT ( 'NONE', #15290 ) ;
#11017 = VERTEX_POINT ( 'NONE', #9397 ) ;
#11018 = VERTEX_POINT ( 'NONE', #8089 ) ;
#11019 = CARTESIAN_POINT ( 'NONE',  ( 10.10406781373725771, 10.99999970914572778, 69.08979243323354069 ) ) ;
#11020 = CARTESIAN_POINT ( 'NONE',  ( -1.418005212499557466, -2.272500000000021281, 3.426931839692804349 ) ) ;
#11021 = TOROIDAL_SURFACE ( 'NONE', #11011, 3.299999999999470024, 0.2000000000005275058 ) ;
#11022 =( NAMED_UNIT ( * ) SI_UNIT ( $, .STERADIAN. ) SOLID_ANGLE_UNIT ( ) );
#11023 = CIRCLE ( 'NONE', #4336, 0.2000000000005226763 ) ;
#11024 = CARTESIAN_POINT ( 'NONE',  ( -2.938526230868574896, -4.390625000000237144, -2.412868667173103443 ) ) ;
#11025 = CARTESIAN_POINT ( 'NONE',  ( -12.81835358098578403, -12.50000029085423847, -8.775548064764199907 ) ) ;
#11026 = EDGE_CURVE ( 'NONE', #14103, #14684, #14132, .T. ) ;
#11027 = CARTESIAN_POINT ( 'NONE',  ( -48.27438362644000591, 65.17411849586700612, -145.4984795835769660 ) ) ;
#11028 = CARTESIAN_POINT ( 'NONE',  ( 1.916065064279496746E-15, 7.362499999999997158, 0.000000000000000000 ) ) ;
#11029 = LINE ( 'NONE', #14431, #13725 ) ;
#11030 = CARTESIAN_POINT ( 'NONE',  ( 17.12895037488186389, 3.654026927208769315, 0.2687305842673423095 ) ) ;
#11031 = DIRECTION ( 'NONE',  ( 0.000000000000000000, 0.000000000000000000, 1.000000000000000000 ) ) ;
#11032 = DIRECTION ( 'NONE',  ( 1.000000000000000000, 0.000000000000000000, 0.000000000000000000 ) ) ;
#11033 = ORIENTED_EDGE ( 'NONE', *, *, #6501, .T. ) ;
#11034 = DIRECTION ( 'NONE',  ( 0.000000000000000000, 0.000000000000000000, 1.000000000000000000 ) ) ;
#11035 = COLOUR_RGB ( '', 0.66274510, 0.83137255, 0.94901961) ;
#11036 = VERTEX_POINT ( 'NONE', #13071 ) ;
#11037 = CIRCLE ( 'NONE', #8563, 17.00000000000000000 ) ;
#11038 = EDGE_LOOP ( 'NONE', ( #11547, #6888 ) ) ;
#11039 = ORIENTED_EDGE ( 'NONE', *, *, #13156, .T. ) ;
#11040 = VECTOR ( 'NONE', #7634, 1000.000000000000000 ) ;
#11041 = CARTESIAN_POINT ( 'NONE',  ( -2.763334307196397166, -5.178749999999838316, 1.847896475581856324 ) ) ;
#11042 = EDGE_CURVE ( 'NONE', #9953, #1111, #4753, .T. ) ;
#11043 = CARTESIAN_POINT ( 'NONE',  ( -86.77438362643999881, 65.17411849586700612, -145.2984795835770058 ) ) ;
#11044 = CARTESIAN_POINT ( 'NONE',  ( 1.260313249030131866, -5.397499999999716636, 3.044840626206112510 ) ) ;
#11045 = CARTESIAN_POINT ( 'NONE',  ( -15.50000000000000000, -1.037157890325000054, -22.50000000000000000 ) ) ;
#11046 = TOROIDAL_SURFACE ( 'NONE', #13034, 1.200000000000000178, 0.6000000000000000888 ) ;
#11047 = PLANE ( 'NONE',  #14161 ) ;
#11048 = EDGE_CURVE ( 'NONE', #13889, #15148, #12985, .T. ) ;
#11049 = CARTESIAN_POINT ( 'NONE',  ( -15.50000000000000000, -0.4000000000005236034, -22.50000000000000000 ) ) ;
#11050 = AXIS2_PLACEMENT_3D ( 'NONE', #6946, #10414, #12761 ) ;
#11051 = DIRECTION ( 'NONE',  ( 0.000000000000000000, 0.000000000000000000, 1.000000000000000000 ) ) ;
#11052 = CARTESIAN_POINT ( 'NONE',  ( -69.77438362644001302, 81.46011849586699327, -81.84847958357697451 ) ) ;
#11053 = CIRCLE ( 'NONE', #14982, 1.785937500000001066 ) ;
#11054 = ADVANCED_FACE ( 'NONE', ( #7096 ), #5536, .F. ) ;
#11055 = CARTESIAN_POINT ( 'NONE',  ( -35.58670980944424400, 5.000000000000001776, 129.5095611191910621 ) ) ;
#11056 = EDGE_CURVE ( 'NONE', #11016, #1481, #14211, .T. ) ;
#11057 = ORIENTED_EDGE ( 'NONE', *, *, #6320, .T. ) ;
#11058 = DIRECTION ( 'NONE',  ( 0.000000000000000000, 0.000000000000000000, 1.000000000000000000 ) ) ;
#11059 = AXIS2_PLACEMENT_3D ( 'NONE', #482, #5217, #14665 ) ;
#11060 = EDGE_LOOP ( 'NONE', ( #8046, #4465, #13281, #4581 ) ) ;
#11061 = AXIS2_PLACEMENT_3D ( 'NONE', #5294, #14660, #7630 ) ;
#11062 = CARTESIAN_POINT ( 'NONE',  ( -80.27438362643999881, 82.17411849586700612, -182.1969643934119745 ) ) ;
#11063 = EDGE_CURVE ( 'NONE', #7989, #4013, #1183, .T. ) ;
#11064 = CARTESIAN_POINT ( 'NONE',  ( 2.275354997129654055, -2.156249999999973799, -3.407984217092054013 ) ) ;
#11065 = ORIENTED_EDGE ( 'NONE', *, *, #11415, .T. ) ;
#11066 = AXIS2_PLACEMENT_3D ( 'NONE', #13937, #8043, #6898 ) ;
#11067 = CARTESIAN_POINT ( 'NONE',  ( -3.630351441462646545, -3.436713562372988306, -1.502189642148185955 ) ) ;
#11068 = CARTESIAN_POINT ( 'NONE',  ( 21.98164641901421135, 11.99999970914576330, -11.73358795631400753 ) ) ;
#11069 = EDGE_CURVE ( 'NONE', #11128, #8406, #14682, .T. ) ;
#11070 = DIRECTION ( 'NONE',  ( 1.000000000000000000, 0.000000000000000000, 0.000000000000000000 ) ) ;
#11071 = AXIS2_PLACEMENT_3D ( 'NONE', #11987, #8640, #6193 ) ;
#11072 = B_SPLINE_CURVE_WITH_KNOTS ( 'NONE', 3,
 ( #8871, #9795, #8710, #12292, #8562, #4148 ),
 .UNSPECIFIED., .F., .F.,
 ( 4, 2, 4 ),
 ( 0.0002380763768130567115, 0.7291065797294590256, 1.457975083082104995 ),
 .UNSPECIFIED. ) ;
#11073 = DIRECTION ( 'NONE',  ( -1.000000000000000000, 0.000000000000000000, 0.000000000000000000 ) ) ;
#11074 = AXIS2_PLACEMENT_3D ( 'NONE', #11173, #6316, #13288 ) ;
#11075 = CARTESIAN_POINT ( 'NONE',  ( -69.77438362644001302, 82.17411849586700612, -80.14847958357698587 ) ) ;
#11076 = DIRECTION ( 'NONE',  ( 0.000000000000000000, 0.000000000000000000, -1.000000000000000000 ) ) ;
#11077 = CYLINDRICAL_SURFACE ( 'NONE', #12790, 0.9999999999999956701 ) ;
#11078 = ORIENTED_EDGE ( 'NONE', *, *, #13048, .F. ) ;
#11079 = EDGE_LOOP ( 'NONE', ( #8613, #13485, #6793, #8841 ) ) ;
#11080 = DIRECTION ( 'NONE',  ( 0.000000000000000000, -0.000000000000000000, -1.000000000000000000 ) ) ;
#11081 = CARTESIAN_POINT ( 'NONE',  ( 0.0009802357451110755779, -1.834999999999918474, -3.766633749593359948 ) ) ;
#11082 = VERTEX_POINT ( 'NONE', #7171 ) ;
#11083 = AXIS2_PLACEMENT_3D ( 'NONE', #10810, #175, #9701 ) ;
#11084 = CIRCLE ( 'NONE', #4390, 8.124999999999992895 ) ;
#11085 = CARTESIAN_POINT ( 'NONE',  ( -56.85838362643999488, 65.17411849586700612, -147.9984795835769944 ) ) ;
#11086 = CARTESIAN_POINT ( 'NONE',  ( -3.461439457045234036, -5.267711698978494894, -0.3686391104329558854 ) ) ;
#11087 = CARTESIAN_POINT ( 'NONE',  ( -91.27438362643999881, 99.17411849586700612, -145.4984795835769660 ) ) ;
#11088 = CARTESIAN_POINT ( 'NONE',  ( -3.696383486563912246, -0.4995676945082690446, -2.108736548924112331 ) ) ;
#11089 = LINE ( 'NONE', #9054, #8234 ) ;
#11090 = DIRECTION ( 'NONE',  ( 0.000000000000000000, 0.000000000000000000, -1.000000000000000000 ) ) ;
#11091 = CARTESIAN_POINT ( 'NONE',  ( -86.77438362643999881, 67.53201699523744139, -147.9984795835769944 ) ) ;
#11092 = VECTOR ( 'NONE', #2960, 1000.000000000000114 ) ;
#11093 = ORIENTED_EDGE ( 'NONE', *, *, #13764, .T. ) ;
#11094 = LINE ( 'NONE', #12565, #14460 ) ;
#11095 = ORIENTED_EDGE ( 'NONE', *, *, #9578, .F. ) ;
#11096 = ORIENTED_EDGE ( 'NONE', *, *, #10242, .F. ) ;
#11097 = VERTEX_POINT ( 'NONE', #11890 ) ;
#11098 = ORIENTED_EDGE ( 'NONE', *, *, #7264, .T. ) ;
#11099 = VERTEX_POINT ( 'NONE', #1253 ) ;
#11100 = CARTESIAN_POINT ( 'NONE',  ( -48.52438362643999881, 65.17411849586700612, -145.4984795835769944 ) ) ;
#11101 = EDGE_CURVE ( 'NONE', #11742, #2988, #14439, .T. ) ;
#11102 = CIRCLE ( 'NONE', #4409, 0.5999999999999998668 ) ;
#11103 = CARTESIAN_POINT ( 'NONE',  ( -1.128754118026385589, -3.703125000000009770, 3.725901868457750954 ) ) ;
#11104 = FACE_OUTER_BOUND ( 'NONE', #1150, .T. ) ;
#11105 = DIRECTION ( 'NONE',  ( 0.000000000000000000, 0.000000000000000000, -1.000000000000000000 ) ) ;
#11106 = DIRECTION ( 'NONE',  ( 1.000000000000000000, 0.000000000000000000, 0.000000000000000000 ) ) ;
#11107 = DIRECTION ( 'NONE',  ( 0.000000000000000000, 0.000000000000000000, 1.000000000000000000 ) ) ;
#11108 = CARTESIAN_POINT ( 'NONE',  ( -52.77438362643999881, 67.53201699523744139, -147.9984795835769944 ) ) ;
#11109 = PLANE ( 'NONE',  #11059 ) ;
#11110 = CARTESIAN_POINT ( 'NONE',  ( -76.48108760497456160, 68.65632084656354550, -83.44847958357698303 ) ) ;
#11111 = VERTEX_POINT ( 'NONE', #6014 ) ;
#11112 = DIRECTION ( 'NONE',  ( 0.000000000000000000, 1.000000000000000000, 0.000000000000000000 ) ) ;
#11113 = ORIENTED_EDGE ( 'NONE', *, *, #438, .F. ) ;
#11114 = VECTOR ( 'NONE', #6051, 1000.000000000000000 ) ;
#11115 = EDGE_LOOP ( 'NONE', ( #484, #4116, #6772, #11165 ) ) ;
#11116 = ORIENTED_EDGE ( 'NONE', *, *, #7727, .T. ) ;
#11117 = CARTESIAN_POINT ( 'NONE',  ( -3.186695398571379734, -5.131874999999967990, 0.9679749472945999855 ) ) ;
#11118 = ADVANCED_FACE ( 'NONE', ( #10722 ), #14064, .T. ) ;
#11119 = CYLINDRICAL_SURFACE ( 'NONE', #529, 1.785937500000001066 ) ;
#11120 = CARTESIAN_POINT ( 'NONE',  ( -1.792750223658541309, -5.928749999999893383, -2.680858111629535578 ) ) ;
#11121 = EDGE_CURVE ( 'NONE', #11427, #3938, #11966, .T. ) ;
#11122 = CARTESIAN_POINT ( 'NONE',  ( -91.02438362644100778, 99.17411849586700612, -182.2484795835770228 ) ) ;
#11123 = LINE ( 'NONE', #7646, #1773 ) ;
#11124 = CARTESIAN_POINT ( 'NONE',  ( 15.50000000000000000, -0.2000000000000000111, -25.80000000297970075 ) ) ;
#11125 = CARTESIAN_POINT ( 'NONE',  ( 10.10045295220800554, -85.69524470659703752, 70.08978589960021566 ) ) ;
#11126 = FACE_OUTER_BOUND ( 'NONE', #5888, .T. ) ;
#11127 = CARTESIAN_POINT ( 'NONE',  ( -86.77438362644100778, 99.17411849586700612, -149.9984795835770228 ) ) ;
#11128 = VERTEX_POINT ( 'NONE', #10807 ) ;
#11129 = DIRECTION ( 'NONE',  ( 0.000000000000000000, 0.000000000000000000, -1.000000000000000000 ) ) ;
#11130 = ADVANCED_FACE ( 'NONE', ( #11737, #4312 ), #9036, .T. ) ;
#11131 = VERTEX_POINT ( 'NONE', #10483 ) ;
#11132 = CARTESIAN_POINT ( 'NONE',  ( -50.73238362643999722, 66.35306774555222376, -147.9984795835769944 ) ) ;
#11133 = CARTESIAN_POINT ( 'NONE',  ( -1.508667427112231785, -3.312499999999990674, -3.644952880303303555 ) ) ;
#11134 = ORIENTED_EDGE ( 'NONE', *, *, #3280, .T. ) ;
#11135 = EDGE_CURVE ( 'NONE', #14025, #8800, #15210, .T. ) ;
#11136 = CARTESIAN_POINT ( 'NONE',  ( -79.02077156573416516, 60.67411849586702743, -73.34256232478206528 ) ) ;
#11137 = CARTESIAN_POINT ( 'NONE',  ( -86.77438362644001302, 99.17411849586700612, -152.4984795835769944 ) ) ;
#11138 = DIRECTION ( 'NONE',  ( 0.000000000000000000, 1.000000000000000000, 0.000000000000000000 ) ) ;
#11139 = EDGE_CURVE ( 'NONE', #9846, #5278, #1420, .T. ) ;
#11140 = DIRECTION ( 'NONE',  ( -1.000000000000000000, 0.000000000000000000, 0.000000000000000000 ) ) ;
#11141 = LINE ( 'NONE', #11294, #15165 ) ;
#11142 = CARTESIAN_POINT ( 'NONE',  ( -13.41835358098578723, 11.39999970914575833, 0.2664120436859911956 ) ) ;
#11143 = DIRECTION ( 'NONE',  ( 0.000000000000000000, 0.000000000000000000, -1.000000000000000000 ) ) ;
#11144 = DIRECTION ( 'NONE',  ( 0.7071067811865425767, -0.000000000000000000, 0.7071067811865525687 ) ) ;
#11145 = VERTEX_POINT ( 'NONE', #242 ) ;
#11146 =( LENGTH_UNIT ( ) NAMED_UNIT ( * ) SI_UNIT ( .MILLI., .METRE. ) );
#11147 = ADVANCED_FACE ( 'NONE', ( #3970 ), #4781, .F. ) ;
#11148 = ORIENTED_EDGE ( 'NONE', *, *, #1091, .F. ) ;
#11149 = DIRECTION ( 'NONE',  ( -1.000000000000000000, 0.000000000000000000, 0.000000000000000000 ) ) ;
#11150 = CARTESIAN_POINT ( 'NONE',  ( 2.697785604507370927, -1.459999999999946008, 2.699193867783729051 ) ) ;
#11151 = ORIENTED_EDGE ( 'NONE', *, *, #667, .F. ) ;
#11152 = ADVANCED_FACE ( 'NONE', ( #12275 ), #2572, .T. ) ;
#11153 = ADVANCED_FACE ( 'NONE', ( #8624 ), #5149, .F. ) ;
#11154 = DIRECTION ( 'NONE',  ( 0.000000000000000000, -1.000000000000000000, 0.000000000000000000 ) ) ;
#11155 = CARTESIAN_POINT ( 'NONE',  ( 57.41329019055577021, 5.000000000000001776, 93.54081111919107627 ) ) ;
#11156 = DIRECTION ( 'NONE',  ( -1.000000000000000000, -2.459952698498907323E-15, 0.000000000000000000 ) ) ;
#11157 = CARTESIAN_POINT ( 'NONE',  ( 1.525801098514460996, -0.4995676945082557219, -3.817740101069251324 ) ) ;
#11158 = CARTESIAN_POINT ( 'NONE',  ( -86.77438362644100778, 99.17411849586700612, -145.2984795835770058 ) ) ;
#11159 = CARTESIAN_POINT ( 'NONE',  ( -14.25000000000000000, -0.2038245569916330158, -23.22168783648699986 ) ) ;
#11160 = LINE ( 'NONE', #5275, #12011 ) ;
#11161 = EDGE_LOOP ( 'NONE', ( #6457, #3472 ) ) ;
#11162 = DIRECTION ( 'NONE',  ( 0.000000000000000000, 1.000000000000000000, 0.000000000000000000 ) ) ;
#11163 = VERTEX_POINT ( 'NONE', #9859 ) ;
#11164 = ORIENTED_EDGE ( 'NONE', *, *, #13793, .F. ) ;
#11165 = ORIENTED_EDGE ( 'NONE', *, *, #1144, .F. ) ;
#11166 = VERTEX_POINT ( 'NONE', #9627 ) ;
#11167 = ORIENTED_EDGE ( 'NONE', *, *, #6216, .F. ) ;
#11168 = CARTESIAN_POINT ( 'NONE',  ( -35.58670980944424400, 5.000000000000001776, 125.5408111191910763 ) ) ;
#11169 = CARTESIAN_POINT ( 'NONE',  ( 2.949251946438511407, -1.475624999999980647, 2.418581166398158455 ) ) ;
#11170 = AXIS2_PLACEMENT_3D ( 'NONE', #6651, #3284, #11512 ) ;
#11171 = CARTESIAN_POINT ( 'NONE',  ( -1.460276376564476175, -4.312500000000168754, -3.521769549316223102 ) ) ;
#11172 = DIRECTION ( 'NONE',  ( -0.000000000000000000, 1.000000000000000000, -0.000000000000000000 ) ) ;
#11173 = CARTESIAN_POINT ( 'NONE',  ( -1.006616814747114065E-29, -2.568816543514387226E-44, 0.000000000000000000 ) ) ;
#11174 = DIRECTION ( 'NONE',  ( 1.000000000000000000, 0.000000000000000000, 0.000000000000000000 ) ) ;
#11175 = CARTESIAN_POINT ( 'NONE',  ( 0.8338062855310036658, -0.7812499999999443778, 4.197676506703500010 ) ) ;
#11176 = PLANE ( 'NONE',  #2854 ) ;
#11177 = FACE_OUTER_BOUND ( 'NONE', #4856, .T. ) ;
#11178 = CARTESIAN_POINT ( 'NONE',  ( -86.77438362643999881, 65.17411849586700612, -150.4984795835770228 ) ) ;
#11179 = AXIS2_PLACEMENT_3D ( 'NONE', #3840, #425, #14605 ) ;
#11180 = ORIENTED_EDGE ( 'NONE', *, *, #5370, .F. ) ;
#11181 = SPHERICAL_SURFACE ( 'NONE', #315, 0.8600000000000014300 ) ;
#11182 = ORIENTED_EDGE ( 'NONE', *, *, #3257, .F. ) ;
#11183 = TOROIDAL_SURFACE ( 'NONE', #6492, 2.700000000000000178, 0.2000000000000000111 ) ;
#11184 = VERTEX_POINT ( 'NONE', #11110 ) ;
#11185 = EDGE_LOOP ( 'NONE', ( #915, #523, #14420, #14107, #14154, #6700 ) ) ;
#11186 = UNCERTAINTY_MEASURE_WITH_UNIT (LENGTH_MEASURE( 1.000000000000000082E-05 ), #4631, 'distance_accuracy_value', 'NONE');
#11187 = CARTESIAN_POINT ( 'NONE',  ( -69.77438362644001302, 82.17411849586700612, -44.99847958359270450 ) ) ;
#11188 = CARTESIAN_POINT ( 'NONE',  ( -3.191126515704095556, -6.069374228118336490, -0.3131016245760979699 ) ) ;
#11189 = VECTOR ( 'NONE', #6799, 999.9999999999998863 ) ;
#11190 = DIRECTION ( 'NONE',  ( 0.5000000000000003331, 0.8660254037844384856, 0.000000000000000000 ) ) ;
#11191 = CARTESIAN_POINT ( 'NONE',  ( -56.85838362644099675, 99.17411849586700612, -147.9984795835769944 ) ) ;
#11192 = DIRECTION ( 'NONE',  ( 0.000000000000000000, 0.000000000000000000, -1.000000000000000000 ) ) ;
#11193 = PLANE ( 'NONE',  #1188 ) ;
#11194 = DIRECTION ( 'NONE',  ( 0.000000000000000000, 1.000000000000000000, 0.000000000000000000 ) ) ;
#11195 = VECTOR ( 'NONE', #1141, 1000.000000000000000 ) ;
#11196 = ADVANCED_FACE ( 'NONE', ( #2657, #4053 ), #12050, .T. ) ;
#11197 = CARTESIAN_POINT ( 'NONE',  ( 2.642398951855386535, -4.475625000000026610, 2.166914421091147069 ) ) ;
#11198 = ORIENTED_EDGE ( 'NONE', *, *, #230, .T. ) ;
#11199 = CARTESIAN_POINT ( 'NONE',  ( 22.58164641901421632, 11.39999970914576188, -8.183940086454237317 ) ) ;
#11200 = EDGE_CURVE ( 'NONE', #7389, #6830, #12846, .T. ) ;
#11201 = CIRCLE ( 'NONE', #14895, 4.500000000000003553 ) ;
#11202 = ORIENTED_EDGE ( 'NONE', *, *, #5804, .T. ) ;
#11203 = DIRECTION ( 'NONE',  ( -0.7071067811865474617, 8.659560562354921765E-17, 0.7071067811865474617 ) ) ;
#11204 = CARTESIAN_POINT ( 'NONE',  ( 3.808142666863014281, -3.046875000000033751, -1.156701755244785801 ) ) ;
#11205 = ORIENTED_EDGE ( 'NONE', *, *, #6437, .T. ) ;
#11206 = AXIS2_PLACEMENT_3D ( 'NONE', #2184, #11731, #7 ) ;
#11207 = DIRECTION ( 'NONE',  ( 1.000000000000000000, 0.000000000000000000, 0.000000000000000000 ) ) ;
#11208 = DIRECTION ( 'NONE',  ( -0.9999934663667179313, 1.567696289299852414E-18, -0.003614861529252313445 ) ) ;
#11209 =( GEOMETRIC_REPRESENTATION_CONTEXT ( 3 ) GLOBAL_UNCERTAINTY_ASSIGNED_CONTEXT ( ( #2815 ) ) GLOBAL_UNIT_ASSIGNED_CONTEXT ( ( #7825, #5272, #6897 ) ) REPRESENTATION_CONTEXT ( 'NONE', 'WORKASPACE' ) );
#11210 = CARTESIAN_POINT ( 'NONE',  ( -57.02438362644099357, 99.17411849586700612, -149.9984795835770228 ) ) ;
#11211 = ADVANCED_FACE ( 'NONE', ( #9778 ), #7477, .F. ) ;
#11212 = EDGE_CURVE ( 'NONE', #12871, #12429, #5549, .T. ) ;
#11213 = CARTESIAN_POINT ( 'NONE',  ( -77.52077156573416516, 0.000000000000000000, -152.4984795835769944 ) ) ;
#11214 = LINE ( 'NONE', #14619, #8255 ) ;
#11215 = FACE_OUTER_BOUND ( 'NONE', #4669, .T. ) ;
#11216 = CARTESIAN_POINT ( 'NONE',  ( -69.19455825983806108, 98.16615590796850199, -94.68115879786580535 ) ) ;
#11217 = VECTOR ( 'NONE', #9446, 1000.000000000000114 ) ;
#11218 = ADVANCED_FACE ( 'NONE', ( #8779 ), #3546, .F. ) ;
#11219 = DIRECTION ( 'NONE',  ( 1.000000000000000000, 2.459952698498907718E-15, 0.000000000000000000 ) ) ;
#11220 = ORIENTED_EDGE ( 'NONE', *, *, #3425, .F. ) ;
#11221 = ORIENTED_EDGE ( 'NONE', *, *, #7472, .F. ) ;
#11222 = CONICAL_SURFACE ( 'NONE', #1806, 2.042000000000002036, 1.047197551196596965 ) ;
#11223 = CARTESIAN_POINT ( 'NONE',  ( 11.02372356922131758, 11.99999970914572955, 69.09311688316493871 ) ) ;
#11224 = CARTESIAN_POINT ( 'NONE',  ( -3.705025434593251621, -1.038125000000020393, -1.124966067554212801 ) ) ;
#11225 = ORIENTED_EDGE ( 'NONE', *, *, #1161, .F. ) ;
#11226 = EDGE_CURVE ( 'NONE', #14843, #1405, #1718, .T. ) ;
#11227 = EDGE_CURVE ( 'NONE', #8717, #6563, #3583, .T. ) ;
#11228 = AXIS2_PLACEMENT_3D ( 'NONE', #6725, #11442, #3068 ) ;
#11229 = DIRECTION ( 'NONE',  ( 0.000000000000000000, 0.000000000000000000, -1.000000000000000000 ) ) ;
#11230 = VECTOR ( 'NONE', #10465, 1000.000000000000000 ) ;
#11231 = CARTESIAN_POINT ( 'NONE',  ( -2.612410911831650306, -5.223873800609857732, -2.385990627414828147 ) ) ;
#11232 = ADVANCED_FACE ( 'NONE', ( #173 ), #14362, .F. ) ;
#11233 = CARTESIAN_POINT ( 'NONE',  ( -69.77438362644001302, 82.17411849586700612, -183.7533135795160320 ) ) ;
#11234 = AXIS2_PLACEMENT_3D ( 'NONE', #11012, #7455, #8608 ) ;
#11235 = DIRECTION ( 'NONE',  ( 0.000000000000000000, 0.000000000000000000, 1.000000000000000000 ) ) ;
#11236 = PLANE ( 'NONE',  #14173 ) ;
#11237 = PLANE ( 'NONE',  #7099 ) ;
#11238 = EDGE_CURVE ( 'NONE', #1706, #13129, #7988, .T. ) ;
#11239 = DIRECTION ( 'NONE',  ( 0.8660254037844383745, -0.5000000000000003331, 0.000000000000000000 ) ) ;
#11240 = EDGE_CURVE ( 'NONE', #4720, #3939, #11910, .T. ) ;
#11241 = ORIENTED_EDGE ( 'NONE', *, *, #5170, .T. ) ;
#11242 = DIRECTION ( 'NONE',  ( 0.8660254037844482555, 0.000000000000000000, -0.4999999999999831801 ) ) ;
#11243 = AXIS2_PLACEMENT_3D ( 'NONE', #6396, #2489, #11107 ) ;
#11244 = VECTOR ( 'NONE', #2477, 1000.000000000000000 ) ;
#11245 = VERTEX_POINT ( 'NONE', #3036 ) ;
#11246 = ORIENTED_EDGE ( 'NONE', *, *, #249, .F. ) ;
#11247 = ORIENTED_EDGE ( 'NONE', *, *, #2512, .F. ) ;
#11248 = ORIENTED_EDGE ( 'NONE', *, *, #10822, .T. ) ;
#11249 = ORIENTED_EDGE ( 'NONE', *, *, #11238, .F. ) ;
#11250 = CARTESIAN_POINT ( 'NONE',  ( -86.77438362643999881, 65.17411849586700612, -182.2484795835770228 ) ) ;
#11251 = EDGE_CURVE ( 'NONE', #6571, #3303, #9742, .T. ) ;
#11252 = CARTESIAN_POINT ( 'NONE',  ( -3.160451915950723389, -4.406249999999939604, -2.110071460981538749 ) ) ;
#11253 = CIRCLE ( 'NONE', #12000, 4.249999999999996447 ) ;
#11254 = CARTESIAN_POINT ( 'NONE',  ( 21.98164641901421135, 11.39999970914576011, -8.183940086454237317 ) ) ;
#11255 = AXIS2_PLACEMENT_3D ( 'NONE', #13717, #6739, #4248 ) ;
#11256 = EDGE_CURVE ( 'NONE', #14071, #8700, #15042, .T. ) ;
#11257 = CARTESIAN_POINT ( 'NONE',  ( 15.50000000000000000, -5.000000000000000000, 26.00000000000000000 ) ) ;
#11258 = CARTESIAN_POINT ( 'NONE',  ( -9.503456061879928640, -12.00000029085427222, 69.60114695342350899 ) ) ;
#11259 = CARTESIAN_POINT ( 'NONE',  ( 0.001121683909886545937, -1.249999999999918066, -4.217678074926116238 ) ) ;
#11260 = LINE ( 'NONE', #10083, #8553 ) ;
#11261 = DIRECTION ( 'NONE',  ( 0.000000000000000000, 1.000000000000000000, 0.000000000000000000 ) ) ;
#11262 = DIRECTION ( 'NONE',  ( -0.8660254037844381525, 0.000000000000000000, -0.5000000000000007772 ) ) ;
#11263 = SHAPE_REPRESENTATION ( 'Sliding Jaws', ( #285 ), #2528 ) ;
#11264 = EDGE_LOOP ( 'NONE', ( #9517, #5678, #6567, #12261 ) ) ;
#11265 = CARTESIAN_POINT ( 'NONE',  ( -86.77438362643999881, 62.81621999649657084, -150.4984795835770228 ) ) ;
#11266 = ORIENTED_EDGE ( 'NONE', *, *, #4909, .F. ) ;
#11267 = ORIENTED_EDGE ( 'NONE', *, *, #6023, .T. ) ;
#11268 = ORIENTED_EDGE ( 'NONE', *, *, #15097, .F. ) ;
#11269 = CIRCLE ( 'NONE', #1598, 1.250000000000001110 ) ;
#11270 = CIRCLE ( 'NONE', #4571, 4.500000000000003553 ) ;
#11271 = CONICAL_SURFACE ( 'NONE', #6331, 3.968749999999992895, 0.7155849933176756661 ) ;
#11272 = CARTESIAN_POINT ( 'NONE',  ( -14.25000000000000000, -2.500000000000000000, 23.22168783648699986 ) ) ;
#11273 = CARTESIAN_POINT ( 'NONE',  ( -3.268702447147800783, -5.116250000000009734, 0.6493246907702930892 ) ) ;
#11274 = DIRECTION ( 'NONE',  ( 1.000000000000000000, 0.000000000000000000, 0.000000000000000000 ) ) ;
#11275 = PLANE ( 'NONE',  #10177 ) ;
#11276 = CARTESIAN_POINT ( 'NONE',  ( -50.73238362643999722, 65.17411849586700612, -147.9984795835769944 ) ) ;
#11277 = FACE_OUTER_BOUND ( 'NONE', #133, .T. ) ;
#11278 = CARTESIAN_POINT ( 'NONE',  ( -38.27438362644000591, 114.1741184958670061, -67.49847958357700861 ) ) ;
#11279 = AXIS2_PLACEMENT_3D ( 'NONE', #13898, #9160, #8868 ) ;
#11280 = DIRECTION ( 'NONE',  ( 0.000000000000000000, 0.000000000000000000, -1.000000000000000000 ) ) ;
#11281 = VERTEX_POINT ( 'NONE', #3115 ) ;
#11282 = DIRECTION ( 'NONE',  ( 0.8660254037844383745, -0.5000000000000003331, 0.000000000000000000 ) ) ;
#11283 = EDGE_LOOP ( 'NONE', ( #7782, #9646, #5945, #7759 ) ) ;
#11284 = VERTEX_POINT ( 'NONE', #4431 ) ;
#11285 = CARTESIAN_POINT ( 'NONE',  ( 4.043635966909349122, -1.968749999999958034, 0.8028061105223156524 ) ) ;
#11286 = VERTEX_POINT ( 'NONE', #6545 ) ;
#11287 = COLOUR_RGB ( '', 0.40784314, 0.44705882, 0.49803922) ;
#11288 = STYLED_ITEM ( 'NONE', ( #12185 ), #5480 ) ;
#11289 = CARTESIAN_POINT ( 'NONE',  ( 57.41329019055577021, 5.000000000000000000, 127.7236236191910734 ) ) ;
#11290 = EDGE_CURVE ( 'NONE', #9311, #953, #2315, .T. ) ;
#11291 = DIRECTION ( 'NONE',  ( -1.000000000000000000, 0.000000000000000000, 0.000000000000000000 ) ) ;
#11292 = LINE ( 'NONE', #1820, #12710 ) ;
#11293 = CARTESIAN_POINT ( 'NONE',  ( 2.573385150445055114, -3.618985300545106920, 6.000000000000001776 ) ) ;
#11294 = CARTESIAN_POINT ( 'NONE',  ( -49.02438362643999881, 65.17411849586700612, -150.4984795835770228 ) ) ;
#11295 = FACE_OUTER_BOUND ( 'NONE', #13944, .T. ) ;
#11296 = AXIS2_PLACEMENT_3D ( 'NONE', #8721, #14538, #13469 ) ;
#11297 = CARTESIAN_POINT ( 'NONE',  ( -14.25000000000000000, -2.500000000000000000, -21.77831216351300014 ) ) ;
#11298 = SPHERICAL_SURFACE ( 'NONE', #7000, 0.6000000000000000888 ) ;
#11299 = ORIENTED_EDGE ( 'NONE', *, *, #1746, .F. ) ;
#11300 = DIRECTION ( 'NONE',  ( 1.000000000000000000, 0.000000000000000000, 0.000000000000000000 ) ) ;
#11301 = CARTESIAN_POINT ( 'NONE',  ( 1.112125432426072313, -1.381875000000161391, 3.661359949638919087 ) ) ;
#11302 = VERTEX_POINT ( 'NONE', #12727 ) ;
#11303 = EDGE_CURVE ( 'NONE', #9479, #8420, #10315, .T. ) ;
#11304 = CARTESIAN_POINT ( 'NONE',  ( -69.77438362644001302, 71.97411849586700328, -80.14847958357698587 ) ) ;
#11305 = ADVANCED_FACE ( 'NONE', ( #14964 ), #12511, .F. ) ;
#11306 = VECTOR ( 'NONE', #2341, 1000.000000000000000 ) ;
#11307 = CIRCLE ( 'NONE', #13309, 4.500000000000003553 ) ;
#11308 = CARTESIAN_POINT ( 'NONE',  ( -53.27438362644000591, 82.17411849586700612, -152.4984795835769944 ) ) ;
#11309 = DIRECTION ( 'NONE',  ( 0.000000000000000000, 0.000000000000000000, 1.000000000000000000 ) ) ;
#11310 = SURFACE_STYLE_FILL_AREA ( #6598 ) ;
#11311 = DIRECTION ( 'NONE',  ( 0.000000000000000000, 1.000000000000000000, 0.000000000000000000 ) ) ;
#11312 = LINE ( 'NONE', #6521, #6504 ) ;
#11313 = EDGE_LOOP ( 'NONE', ( #3656, #1593, #6652, #10919 ) ) ;
#11314 = CARTESIAN_POINT ( 'NONE',  ( -52.77438362643999881, 65.17411849586700612, -147.9984795835769944 ) ) ;
#11315 = CONICAL_SURFACE ( 'NONE', #13790, 4.500000000000000888, 1.396263401595466691 ) ;
#11316 = VERTEX_POINT ( 'NONE', #2015 ) ;
#11317 = VECTOR ( 'NONE', #12624, 1000.000000000000000 ) ;
#11318 = VERTEX_POINT ( 'NONE', #8928 ) ;
#11319 = EDGE_LOOP ( 'NONE', ( #1238, #3366, #5690, #14577 ) ) ;
#11320 = ORIENTED_EDGE ( 'NONE', *, *, #9886, .F. ) ;
#11321 = EDGE_CURVE ( 'NONE', #10418, #9704, #3559, .T. ) ;
#11322 = VERTEX_POINT ( 'NONE', #12649 ) ;
#11323 = CARTESIAN_POINT ( 'NONE',  ( -0.6922063445227994993, -6.280463562373093112, -3.484636965811530818 ) ) ;
#11324 = CARTESIAN_POINT ( 'NONE',  ( 0.001402937982463629916, -1.335000000000034825, 3.832736870811212171 ) ) ;
#11325 = EDGE_CURVE ( 'NONE', #2361, #9205, #8265, .T. ) ;
#11326 = EDGE_CURVE ( 'NONE', #13856, #12032, #4355, .T. ) ;
#11327 = CARTESIAN_POINT ( 'NONE',  ( -104.2743836264399988, 111.1741184958670061, -67.49847958357700861 ) ) ;
#11328 = CARTESIAN_POINT ( 'NONE',  ( -3.978302601493375334, -2.468750000000105693, -0.7924256976418916354 ) ) ;
#11329 = CARTESIAN_POINT ( 'NONE',  ( -66.62325245518700001, 97.86074886511960358, -93.49847958357699440 ) ) ;
#11330 = DIRECTION ( 'NONE',  ( 0.000000000000000000, 0.000000000000000000, -1.000000000000000000 ) ) ;
#11331 = CIRCLE ( 'NONE', #9342, 3.299999999999473577 ) ;
#11332 = CARTESIAN_POINT ( 'NONE',  ( -2.598076211353319565, 1.678847577293365978, -4.499999999999999112 ) ) ;
#11333 = CARTESIAN_POINT ( 'NONE',  ( -1.243836315904764955, -0.7031249999999807931, 4.105705763534058583 ) ) ;
#11334 = DIRECTION ( 'NONE',  ( 0.000000000000000000, 1.000000000000000000, 0.000000000000000000 ) ) ;
#11335 = DIRECTION ( 'NONE',  ( 0.000000000000000000, 0.000000000000000000, 1.000000000000000000 ) ) ;
#11336 = CARTESIAN_POINT ( 'NONE',  ( -52.77438362644000591, 99.17411849586700612, -79.59847958357700293 ) ) ;
#11337 = EDGE_CURVE ( 'NONE', #11166, #13163, #8582, .T. ) ;
#11338 = ORIENTED_EDGE ( 'NONE', *, *, #4, .T. ) ;
#11339 = DIRECTION ( 'NONE',  ( 1.000000000000000000, -0.000000000000000000, 0.000000000000000000 ) ) ;
#11340 = ORIENTED_EDGE ( 'NONE', *, *, #12258, .F. ) ;
#11341 = ORIENTED_EDGE ( 'NONE', *, *, #7465, .F. ) ;
#11342 = VERTEX_POINT ( 'NONE', #9002 ) ;
#11343 = UNCERTAINTY_MEASURE_WITH_UNIT (LENGTH_MEASURE( 1.000000000000000082E-05 ), #10918, 'distance_accuracy_value', 'NONE');
#11344 = EDGE_CURVE ( 'NONE', #9860, #12733, #11488, .T. ) ;
#11345 = CIRCLE ( 'NONE', #1681, 4.000000000000000000 ) ;
#11346 = CARTESIAN_POINT ( 'NONE',  ( -52.77438362644000591, 99.17411849586700612, -152.4984795835769944 ) ) ;
#11347 = CARTESIAN_POINT ( 'NONE',  ( 0.3227798623957477964, -5.350624999999817888, 3.285751646651179136 ) ) ;
#11348 = EDGE_CURVE ( 'NONE', #13148, #2388, #9485, .T. ) ;
#11349 = EDGE_CURVE ( 'NONE', #15330, #9916, #10221, .T. ) ;
#11350 = CARTESIAN_POINT ( 'NONE',  ( -4.522482571421201136, -12.00000029085427222, 70.03692566716181034 ) ) ;
#11351 = CARTESIAN_POINT ( 'NONE',  ( -65.90140028023573393, 75.17411849586525818, -44.99847958359791278 ) ) ;
#11352 = DIRECTION ( 'NONE',  ( 0.000000000000000000, 0.000000000000000000, 1.000000000000000000 ) ) ;
#11353 = FACE_OUTER_BOUND ( 'NONE', #4940, .T. ) ;
#11354 = CARTESIAN_POINT ( 'NONE',  ( 1.002467944199222138, -0.4995676945082564990, 3.916338062624285410 ) ) ;
#11355 = CARTESIAN_POINT ( 'NONE',  ( -86.77438362644100778, 99.17411849586700612, -146.8195303338917768 ) ) ;
#11356 = DIRECTION ( 'NONE',  ( 0.000000000000000000, 0.000000000000000000, -1.000000000000000000 ) ) ;
#11357 = EDGE_LOOP ( 'NONE', ( #10337, #11779, #2081 ) ) ;
#11358 = CARTESIAN_POINT ( 'NONE',  ( -73.64736697264743270, 75.17411849586699191, -58.99847958357700151 ) ) ;
#11359 = ORIENTED_EDGE ( 'NONE', *, *, #1916, .T. ) ;
#11360 = VERTEX_POINT ( 'NONE', #8856 ) ;
#11361 = CARTESIAN_POINT ( 'NONE',  ( -4.184567129761759929, -1.500000000000142109, 0.001513272625389735625 ) ) ;
#11362 = ORIENTED_EDGE ( 'NONE', *, *, #2125, .F. ) ;
#11363 = B_SPLINE_CURVE_WITH_KNOTS ( 'NONE', 3,
 ( #12324, #1833, #669, #4243 ),
 .UNSPECIFIED., .F., .F.,
 ( 4, 4 ),
 ( 0.000000000000000000, 0.0004098597307629696612 ),
 .UNSPECIFIED. ) ;
#11364 = CARTESIAN_POINT ( 'NONE',  ( -2.167558509990396232, -3.655463562373140185, 3.242140913184852202 ) ) ;
#11365 = CIRCLE ( 'NONE', #9873, 1.785937500000001066 ) ;
#11366 = LINE ( 'NONE', #7664, #15126 ) ;
#11367 = DIRECTION ( 'NONE',  ( 0.000000000000000000, 0.000000000000000000, 1.000000000000000000 ) ) ;
#11368 = DIRECTION ( 'NONE',  ( 1.000000000000000000, 0.000000000000000000, 0.000000000000000000 ) ) ;
#11369 = DIRECTION ( 'NONE',  ( 0.000000000000000000, 0.000000000000000000, -1.000000000000000000 ) ) ;
#11370 = DIRECTION ( 'NONE',  ( 0.4999999999999998890, -0.8660254037844387076, 0.000000000000000000 ) ) ;
#11371 = CARTESIAN_POINT ( 'NONE',  ( -50.07438362643999596, 65.17411849586700612, -145.4984795835769944 ) ) ;
#11372 = CARTESIAN_POINT ( 'NONE',  ( -52.77438362644100067, 99.17411849586700612, -145.2984795835770058 ) ) ;
#11373 = ORIENTED_EDGE ( 'NONE', *, *, #1398, .F. ) ;
#11374 = DIRECTION ( 'NONE',  ( 0.000000000000000000, 0.000000000000000000, 1.000000000000000000 ) ) ;
#11375 = CARTESIAN_POINT ( 'NONE',  ( 0.7224497989600291437, -2.366250000000003517, 3.625028471221729554 ) ) ;
#11376 = ORIENTED_EDGE ( 'NONE', *, *, #5844, .F. ) ;
#11377 = DIRECTION ( 'NONE',  ( 0.000000000000000000, 1.000000000000000000, 0.000000000000000000 ) ) ;
#11378 = DIRECTION ( 'NONE',  ( -0.000000000000000000, 1.000000000000000000, -0.000000000000000000 ) ) ;
#11379 = DIRECTION ( 'NONE',  ( 0.000000000000000000, 0.000000000000000000, 1.000000000000000000 ) ) ;
#11380 = DIRECTION ( 'NONE',  ( 0.000000000000000000, -1.000000000000000000, -4.336808689942017736E-16 ) ) ;
#11381 = LINE ( 'NONE', #7963, #3358 ) ;
#11382 = EDGE_CURVE ( 'NONE', #3615, #1459, #5800, .T. ) ;
#11383 = DIRECTION ( 'NONE',  ( 0.000000000000000000, 0.000000000000000000, -1.000000000000000000 ) ) ;
#11384 = EDGE_LOOP ( 'NONE', ( #10576, #10747 ) ) ;
#11385 = FACE_OUTER_BOUND ( 'NONE', #10626, .T. ) ;
#11386 = EDGE_CURVE ( 'NONE', #5234, #5837, #5836, .T. ) ;
#11387 = ORIENTED_EDGE ( 'NONE', *, *, #799, .T. ) ;
#11388 = VERTEX_POINT ( 'NONE', #9381 ) ;
#11389 = CARTESIAN_POINT ( 'NONE',  ( 0.3183433322350087691, -5.819374999999986642, -3.223879781222068086 ) ) ;
#11390 = VERTEX_POINT ( 'NONE', #7074 ) ;
#11391 = ORIENTED_EDGE ( 'NONE', *, *, #4513, .T. ) ;
#11392 = B_SPLINE_CURVE_WITH_KNOTS ( 'NONE', 3,
 ( #15038, #3111, #7848, #6762, #4496, #15186, #12720, #9076, #11482, #9299, #4427, #9147 ),
 .UNSPECIFIED., .F., .F.,
 ( 4, 2, 2, 2, 2, 4 ),
 ( 2.544323688695237330E-07, 0.001342108318545693138, 0.002013035261634103963, 0.002683962204722515222, 0.004025816090899335571, 0.005367669977076155487 ),
 .UNSPECIFIED. ) ;
#11393 = ORIENTED_EDGE ( 'NONE', *, *, #7251, .F. ) ;
#11394 = CARTESIAN_POINT ( 'NONE',  ( -2.735908675276634838, -6.389838562373163278, -2.243606804512522146 ) ) ;
#11395 = CARTESIAN_POINT ( 'NONE',  ( 2.123627735229571822, -1.428750000000023501, 3.175715285003293253 ) ) ;
#11396 = DIRECTION ( 'NONE',  ( 1.000000000000000000, 0.000000000000000000, 0.000000000000000000 ) ) ;
#11397 = CARTESIAN_POINT ( 'NONE',  ( 2.275354997129654055, -2.156249999999973799, -3.407984217092054013 ) ) ;
#11398 = CARTESIAN_POINT ( 'NONE',  ( -57.27438362644000591, 65.17411849586700612, -152.4984795835769944 ) ) ;
#11399 = CYLINDRICAL_SURFACE ( 'NONE', #8628, 1.999999999999988010 ) ;
#11400 = CARTESIAN_POINT ( 'NONE',  ( -3.579691249134443698, -0.5937499999999900080, 2.390491442833416080 ) ) ;
#11401 = DIRECTION ( 'NONE',  ( 0.000000000000000000, 1.000000000000000000, 0.000000000000000000 ) ) ;
#11402 = EDGE_CURVE ( 'NONE', #4340, #15166, #4960, .T. ) ;
#11403 = CARTESIAN_POINT ( 'NONE',  ( 57.41329019055577021, 2.488961461112888074, 97.50956111919106206 ) ) ;
#11404 = DIRECTION ( 'NONE',  ( 1.000000000000000000, 0.000000000000000000, 0.000000000000000000 ) ) ;
#11405 = ORIENTED_EDGE ( 'NONE', *, *, #2411, .T. ) ;
#11406 = CARTESIAN_POINT ( 'NONE',  ( -59.27438362644000591, 82.17411849586700612, -80.14847958357698587 ) ) ;
#11407 = EDGE_CURVE ( 'NONE', #4297, #7989, #14198, .T. ) ;
#11408 = EDGE_LOOP ( 'NONE', ( #14537, #6679 ) ) ;
#11409 = ORIENTED_EDGE ( 'NONE', *, *, #11826, .T. ) ;
#11410 = ORIENTED_EDGE ( 'NONE', *, *, #8692, .T. ) ;
#11411 = B_SPLINE_CURVE_WITH_KNOTS ( 'NONE', 3,
 ( #1308, #8299, #6153, #10861 ),
 .UNSPECIFIED., .F., .F.,
 ( 4, 4 ),
 ( 0.01442070979368249156, 0.01702197257837674560 ),
 .UNSPECIFIED. ) ;
#11412 = PLANE ( 'NONE',  #4767 ) ;
#11413 = B_SPLINE_CURVE_WITH_KNOTS ( 'NONE', 3,
 ( #7124, #2449, #2085, #6836, #10667, #118, #13247, #10756, #2372, #42, #2605, #7200, #4784, #1447, #6127, #4870, #198, #11558, #922, #11844, #12716, #5017, #6203, #15103 ),
 .UNSPECIFIED., .F., .F.,
 ( 4, 2, 2, 2, 2, 2, 2, 2, 2, 2, 2, 4 ),
 ( 0.000000000000000000, 0.0008863986295625844031, 0.001329597944343876821, 0.001772797259125169240, 0.002659195888687754077, 0.003102395203469047145, 0.003545594518250340214, 0.004431993147812924617, 0.005318391777375509888, 0.005761591092156802089, 0.006204790406938094291, 0.007091189036500678694 ),
 .UNSPECIFIED. ) ;
#11414 = CARTESIAN_POINT ( 'NONE',  ( 0.9968050443165101804, -4.381875000000003517, 3.281628308787421400 ) ) ;
#11415 = EDGE_CURVE ( 'NONE', #11629, #13427, #1083, .T. ) ;
#11416 = FACE_BOUND ( 'NONE', #12852, .T. ) ;
#11417 = EDGE_CURVE ( 'NONE', #10624, #2361, #2245, .T. ) ;
#11418 = PLANE ( 'NONE',  #7249 ) ;
#11419 = CARTESIAN_POINT ( 'NONE',  ( -86.77438362644001302, 99.17411849586700612, -152.4984795835769944 ) ) ;
#11420 = AXIS2_PLACEMENT_3D ( 'NONE', #12069, #1508, #8489 ) ;
#11421 = DIRECTION ( 'NONE',  ( -1.000000000000000000, 0.000000000000000000, 0.000000000000000000 ) ) ;
#11422 = DIRECTION ( 'NONE',  ( 1.000000000000000000, 0.000000000000000000, 0.000000000000000000 ) ) ;
#11423 = LINE ( 'NONE', #4522, #14479 ) ;
#11424 = EDGE_CURVE ( 'NONE', #10300, #777, #7035, .T. ) ;
#11425 = CIRCLE ( 'NONE', #7482, 2.699999999999993960 ) ;
#11426 = CARTESIAN_POINT ( 'NONE',  ( 3.136514378097080780, -4.647499999999995524, -1.298252083346796759 ) ) ;
#11427 = VERTEX_POINT ( 'NONE', #6919 ) ;
#11428 = CARTESIAN_POINT ( 'NONE',  ( -88.81638362644000040, 65.17411849586700612, -147.9984795835769944 ) ) ;
#11429 = EDGE_CURVE ( 'NONE', #15067, #4543, #15271, .T. ) ;
#11430 = ORIENTED_EDGE ( 'NONE', *, *, #7169, .F. ) ;
#11431 = EDGE_CURVE ( 'NONE', #6301, #6290, #3414, .T. ) ;
#11432 = CARTESIAN_POINT ( 'NONE',  ( -69.77438362644001302, 82.17411849586700612, -81.84847958357698872 ) ) ;
#11433 = ORIENTED_EDGE ( 'NONE', *, *, #5666, .F. ) ;
#11434 = CIRCLE ( 'NONE', #13183, 3.300000002979700753 ) ;
#11435 = CARTESIAN_POINT ( 'NONE',  ( 0.8105829119240891556, -1.781250000000002887, 4.067378511145360420 ) ) ;
#11436 = ORIENTED_EDGE ( 'NONE', *, *, #12964, .F. ) ;
#11437 = CARTESIAN_POINT ( 'NONE',  ( 3.809485474318313081, -3.046088562373004738, -1.154500326837077484 ) ) ;
#11438 = CIRCLE ( 'NONE', #9686, 2.042000000000002036 ) ;
#11439 = CARTESIAN_POINT ( 'NONE',  ( -1.096602777094355814E-14, 4.297149196226271783, 0.000000000000000000 ) ) ;
#11440 = CIRCLE ( 'NONE', #13433, 17.00000000000000000 ) ;
#11441 = DIRECTION ( 'NONE',  ( 0.000000000000000000, 0.000000000000000000, 1.000000000000000000 ) ) ;
#11442 = DIRECTION ( 'NONE',  ( 0.000000000000000000, 0.000000000000000000, -1.000000000000000000 ) ) ;
#11443 = ADVANCED_FACE ( 'NONE', ( #1003 ), #15112, .F. ) ;
#11444 = VECTOR ( 'NONE', #10475, 1000.000000000000000 ) ;
#11445 = CARTESIAN_POINT ( 'NONE',  ( -1.705466066262326307E-14, 9.560000000000000497, 5.619086434621074034E-29 ) ) ;
#11446 = DIRECTION ( 'NONE',  ( 0.000000000000000000, 1.000000000000000000, 0.000000000000000000 ) ) ;
#11447 = CARTESIAN_POINT ( 'NONE',  ( -69.77438362644001302, 81.46011849586699327, -83.44847958357698303 ) ) ;
#11448 = DIRECTION ( 'NONE',  ( 1.000000000000000000, 0.000000000000000000, 0.000000000000000000 ) ) ;
#11449 = CIRCLE ( 'NONE', #12953, 2.431404194366992400 ) ;
#11450 = DIRECTION ( 'NONE',  ( 0.000000000000000000, 0.000000000000000000, 1.000000000000000000 ) ) ;
#11451 = VERTEX_POINT ( 'NONE', #4500 ) ;
#11452 = DIRECTION ( 'NONE',  ( -1.000000000000000000, 0.000000000000000000, 0.000000000000000000 ) ) ;
#11453 = CARTESIAN_POINT ( 'NONE',  ( 3.768993168962233575, -0.5381249999999744293, 1.141810966380977455 ) ) ;
#11454 = EDGE_LOOP ( 'NONE', ( #5982, #12868 ) ) ;
#11455 = CIRCLE ( 'NONE', #10200, 2.500000000000002220 ) ;
#11456 = CARTESIAN_POINT ( 'NONE',  ( 0.0009802357451226765411, -1.834999999999918474, -3.766633749593359060 ) ) ;
#11457 = DIRECTION ( 'NONE',  ( 1.000000000000000000, 0.000000000000000000, 0.000000000000000000 ) ) ;
#11458 = CYLINDRICAL_SURFACE ( 'NONE', #5145, 4.250000000000003553 ) ;
#11459 = CIRCLE ( 'NONE', #14678, 10.50000000000000178 ) ;
#11460 = PLANE ( 'NONE',  #593 ) ;
#11461 = CARTESIAN_POINT ( 'NONE',  ( -69.77438362644001302, 82.17411849586700612, -93.49847958357699440 ) ) ;
#11462 = DIRECTION ( 'NONE',  ( -0.000000000000000000, 1.000000000000000000, -0.000000000000000000 ) ) ;
#11463 = CARTESIAN_POINT ( 'NONE',  ( 3.469446951953614189E-15, -24.00000000000000000, 0.000000000000000000 ) ) ;
#11464 = CARTESIAN_POINT ( 'NONE',  ( 17.12895037488186389, 11.13833052492975106, 0.2687305842673423095 ) ) ;
#11465 = CIRCLE ( 'NONE', #4536, 8.000000000000007105 ) ;
#11466 = ORIENTED_EDGE ( 'NONE', *, *, #11496, .T. ) ;
#11467 = CARTESIAN_POINT ( 'NONE',  ( -52.77438362644000591, 99.17411849586700612, -86.49847958357699440 ) ) ;
#11468 = ORIENTED_EDGE ( 'NONE', *, *, #8922, .T. ) ;
#11469 = ORIENTED_EDGE ( 'NONE', *, *, #8935, .F. ) ;
#11470 = EDGE_LOOP ( 'NONE', ( #12497, #6789, #568 ) ) ;
#11471 = ORIENTED_EDGE ( 'NONE', *, *, #14659, .F. ) ;
#11472 = CIRCLE ( 'NONE', #8744, 4.499999999999997335 ) ;
#11473 = AXIS2_PLACEMENT_3D ( 'NONE', #15114, #12968, #8227 ) ;
#11474 = ORIENTED_EDGE ( 'NONE', *, *, #8292, .T. ) ;
#11475 = CARTESIAN_POINT ( 'NONE',  ( -1.031947532464913664, -6.296088562372862185, -3.397346913929182755 ) ) ;
#11476 = CARTESIAN_POINT ( 'NONE',  ( -3.795858268372354516, -1.053749999999936460, -0.7536008350790791566 ) ) ;
#11477 = CARTESIAN_POINT ( 'NONE',  ( 40.52020888806953991, 0.000000000000000000, 6.000000000000000000 ) ) ;
#11478 = CARTESIAN_POINT ( 'NONE',  ( -1.920019182618211584, -2.328124999999937383, -3.594387849940205104 ) ) ;
#11479 = CARTESIAN_POINT ( 'NONE',  ( -69.77438362644001302, 82.17411849586700612, -93.49847958357699440 ) ) ;
#11480 = EDGE_CURVE ( 'NONE', #10868, #7835, #3650, .T. ) ;
#11481 = DIRECTION ( 'NONE',  ( 0.000000000000000000, 0.000000000000000000, 1.000000000000000000 ) ) ;
#11482 = CARTESIAN_POINT ( 'NONE',  ( 4.342069816296828755, 2.307268873417431809, 1.479314468162619578 ) ) ;
#11483 = CARTESIAN_POINT ( 'NONE',  ( 3.757405615841324042, -0.9218749999999823475, 2.009662442622283773 ) ) ;
#11484 = CARTESIAN_POINT ( 'NONE',  ( 14.79833345856040694, -1.094824204497501265E-15, 26.90780383552089106 ) ) ;
#11485 = CIRCLE ( 'NONE', #3567, 4.401041666666736241 ) ;
#11486 = FACE_OUTER_BOUND ( 'NONE', #10211, .T. ) ;
#11487 = AXIS2_PLACEMENT_3D ( 'NONE', #8510, #13255, #5978 ) ;
#11488 = LINE ( 'NONE', #853, #6309 ) ;
#11489 = ORIENTED_EDGE ( 'NONE', *, *, #7459, .F. ) ;
#11490 = DIRECTION ( 'NONE',  ( 0.000000000000000000, 0.000000000000000000, -1.000000000000000000 ) ) ;
#11491 = ORIENTED_EDGE ( 'NONE', *, *, #1112, .T. ) ;
#11492 = ORIENTED_EDGE ( 'NONE', *, *, #11026, .F. ) ;
#11493 = ORIENTED_EDGE ( 'NONE', *, *, #7519, .F. ) ;
#11494 = DIRECTION ( 'NONE',  ( -1.000000000000000000, 0.000000000000000000, 0.000000000000000000 ) ) ;
#11495 = CIRCLE ( 'NONE', #5056, 1.785937500000001066 ) ;
#11496 = EDGE_CURVE ( 'NONE', #14868, #7121, #8266, .T. ) ;
#11497 = CARTESIAN_POINT ( 'NONE',  ( 1.879752899984456160, -4.741249999999911147, -2.811701655874830230 ) ) ;
#11498 = VECTOR ( 'NONE', #1541, 1000.000000000000000 ) ;
#11499 = DIRECTION ( 'NONE',  ( 0.000000000000000000, 0.000000000000000000, -1.000000000000000000 ) ) ;
#11500 = CARTESIAN_POINT ( 'NONE',  ( -14.25000000000000000, -2.500000000000000000, -21.77831216351300014 ) ) ;
#11501 = LINE ( 'NONE', #13978, #926 ) ;
#11502 = CARTESIAN_POINT ( 'NONE',  ( -0.7619189956411019926, -0.4995676945082610509, 4.033706137351277476 ) ) ;
#11503 = DIRECTION ( 'NONE',  ( 0.000000000000000000, -1.000000000000000000, -4.336808689942017736E-16 ) ) ;
#11504 = ORIENTED_EDGE ( 'NONE', *, *, #12952, .F. ) ;
#11505 = CYLINDRICAL_SURFACE ( 'NONE', #15279, 0.5999999999999998668 ) ;
#11506 = CLOSED_SHELL ( 'NONE', ( #3527, #15024, #8570, #1592, #13236, #4817, #9226, #2278, #14634, #13484, #6807, #2893, #10770, #12583, #7086, #9389, #4869, #904, #10668, #9880, #711, #3522, #14277, #3262, #10359, #14167 ) ) ;
#11507 = VECTOR ( 'NONE', #7693, 999.9999999999998863 ) ;
#11508 = AXIS2_PLACEMENT_3D ( 'NONE', #10563, #84, #14209 ) ;
#11509 = ORIENTED_EDGE ( 'NONE', *, *, #9810, .F. ) ;
#11510 = EDGE_CURVE ( 'NONE', #1497, #13889, #14118, .T. ) ;
#11511 = VERTEX_POINT ( 'NONE', #9222 ) ;
#11512 = DIRECTION ( 'NONE',  ( 0.000000000000000000, 1.000000000000000000, 0.000000000000000000 ) ) ;
#11513 = ORIENTED_EDGE ( 'NONE', *, *, #11480, .F. ) ;
#11514 = CARTESIAN_POINT ( 'NONE',  ( -3.245221319803801130, -1.390624999999827915, -2.664727821046819489 ) ) ;
#11515 = ORIENTED_EDGE ( 'NONE', *, *, #7749, .T. ) ;
#11516 = ADVANCED_FACE ( 'NONE', ( #12965 ), #13963, .F. ) ;
#11517 = CARTESIAN_POINT ( 'NONE',  ( 1.534191850248811884, -2.811713562373064690, 3.706628987441562995 ) ) ;
#11518 = CARTESIAN_POINT ( 'NONE',  ( 22.58164641901421632, 11.99999970914576863, -56.77834603255778489 ) ) ;
#11519 = EDGE_CURVE ( 'NONE', #2023, #11281, #3300, .T. ) ;
#11520 = DIRECTION ( 'NONE',  ( 0.000000000000000000, 1.000000000000000000, 0.000000000000000000 ) ) ;
#11521 = EDGE_CURVE ( 'NONE', #14726, #8931, #2812, .T. ) ;
#11522 = VECTOR ( 'NONE', #8853, 1000.000000000000000 ) ;
#11523 = LINE ( 'NONE', #3217, #9998 ) ;
#11524 = CARTESIAN_POINT ( 'NONE',  ( -71.19907181086536241, 98.11283521318516421, -94.49649318951415466 ) ) ;
#11525 = PLANE ( 'NONE',  #14670 ) ;
#11526 = EDGE_CURVE ( 'NONE', #5090, #4630, #3571, .T. ) ;
#11527 = APPLICATION_PROTOCOL_DEFINITION ( 'draft international standard', 'automotive_design', 1998, #9108 ) ;
#11528 = ORIENTED_EDGE ( 'NONE', *, *, #6225, .F. ) ;
#11529 = AXIS2_PLACEMENT_3D ( 'NONE', #8993, #8919, #11396 ) ;
#11530 = DIRECTION ( 'NONE',  ( -1.000000000000000000, 0.000000000000000000, 0.000000000000000000 ) ) ;
#11531 = CARTESIAN_POINT ( 'NONE',  ( 3.280408283555247717, -0.4912499999999521139, 2.190169342145847242 ) ) ;
#11532 = EDGE_LOOP ( 'NONE', ( #4686, #88, #1808, #9553, #7060, #1 ) ) ;
#11533 = AXIS2_PLACEMENT_3D ( 'NONE', #8445, #4024, #8752 ) ;
#11534 = ADVANCED_FACE ( 'NONE', ( #930 ), #11983, .T. ) ;
#11535 = CARTESIAN_POINT ( 'NONE',  ( 3.722330097189530562, -1.616249999999942899, -0.7418360188101028596 ) ) ;
#11536 = FACE_OUTER_BOUND ( 'NONE', #12751, .T. ) ;
#11537 = DIRECTION ( 'NONE',  ( 1.000000000000000000, 0.000000000000000000, 0.000000000000000000 ) ) ;
#11538 = VECTOR ( 'NONE', #3590, 1000.000000000000000 ) ;
#11539 = CARTESIAN_POINT ( 'NONE',  ( -54.81638362644100226, 97.99516924618178848, -150.4984795835770228 ) ) ;
#11540 = LINE ( 'NONE', #3163, #10614 ) ;
#11541 = CARTESIAN_POINT ( 'NONE',  ( -52.77438362644100067, 99.17411849586700612, -146.8195303338917768 ) ) ;
#11542 = AXIS2_PLACEMENT_3D ( 'NONE', #2610, #9892, #14620 ) ;
#11543 = DIRECTION ( 'NONE',  ( 0.000000000000000000, 1.000000000000000000, 0.000000000000000000 ) ) ;
#11544 = CARTESIAN_POINT ( 'NONE',  ( 6.573385150445030689, -19.31989681812820692, 6.000000000000000000 ) ) ;
#11545 = VERTEX_POINT ( 'NONE', #223 ) ;
#11546 = CARTESIAN_POINT ( 'NONE',  ( -53.79538362643999960, 66.94254237039483257, -147.9984795835769944 ) ) ;
#11547 = ORIENTED_EDGE ( 'NONE', *, *, #10924, .T. ) ;
#11548 = ORIENTED_EDGE ( 'NONE', *, *, #149, .F. ) ;
#11549 = CARTESIAN_POINT ( 'NONE',  ( 1.903042727507281651, -4.428749999999965326, 2.845810502761935812 ) ) ;
#11550 = ORIENTED_EDGE ( 'NONE', *, *, #2677, .T. ) ;
#11551 = VECTOR ( 'NONE', #13333, 1000.000000000000114 ) ;
#11552 = EDGE_LOOP ( 'NONE', ( #12400, #4456, #13907, #10811, #11909 ) ) ;
#11553 = ORIENTED_EDGE ( 'NONE', *, *, #7430, .F. ) ;
#11554 = AXIS2_PLACEMENT_3D ( 'NONE', #6930, #15285, #4747 ) ;
#11555 = LINE ( 'NONE', #3177, #7300 ) ;
#11556 = VECTOR ( 'NONE', #14974, 1000.000000000000000 ) ;
#11557 = CARTESIAN_POINT ( 'NONE',  ( -3.686556889460864461, -0.1475000000000124822, 1.525885089196999056 ) ) ;
#11558 = CARTESIAN_POINT ( 'NONE',  ( -3.050151834521379168, -5.307756522154472023, 1.562533256231358747 ) ) ;
#11559 = CARTESIAN_POINT ( 'NONE',  ( 2.623679764461153141, -1.859375000000051070, 3.198691315062023310 ) ) ;
#11560 = CARTESIAN_POINT ( 'NONE',  ( -75.19401665569927218, 66.06115545897768015, -81.84847958357697451 ) ) ;
#11561 = DIRECTION ( 'NONE',  ( 0.000000000000000000, -4.336808689942017736E-16, 1.000000000000000000 ) ) ;
#11562 = PLANE ( 'NONE',  #693 ) ;
#11563 = CIRCLE ( 'NONE', #8598, 3.499999999999999556 ) ;
#11564 = FACE_OUTER_BOUND ( 'NONE', #5208, .T. ) ;
#11565 = DIRECTION ( 'NONE',  ( -0.000000000000000000, -0.000000000000000000, 1.000000000000000000 ) ) ;
#11566 = CARTESIAN_POINT ( 'NONE',  ( -88.81638362644100937, 97.99516924618178848, -147.9984795835769944 ) ) ;
#11567 = VECTOR ( 'NONE', #2398, 1000.000000000000114 ) ;
#11568 = VERTEX_POINT ( 'NONE', #6224 ) ;
#11569 = CARTESIAN_POINT ( 'NONE',  ( -15.50000000000000000, -2.500000000000000000, 21.05662432702600029 ) ) ;
#11570 = VERTEX_POINT ( 'NONE', #10932 ) ;
#11571 = EDGE_LOOP ( 'NONE', ( #10373, #6941, #690 ) ) ;
#11572 = EDGE_LOOP ( 'NONE', ( #8284, #7708, #8249, #5482 ) ) ;
#11573 = EDGE_CURVE ( 'NONE', #3973, #9306, #13354, .T. ) ;
#11574 = DIRECTION ( 'NONE',  ( 0.000000000000000000, 0.000000000000000000, 1.000000000000000000 ) ) ;
#11575 = AXIS2_PLACEMENT_3D ( 'NONE', #11766, #14529, #11614 ) ;
#11576 = FACE_OUTER_BOUND ( 'NONE', #1721, .T. ) ;
#11577 = CARTESIAN_POINT ( 'NONE',  ( -69.43626855224094641, 75.17411849586699191, -43.99847958365483436 ) ) ;
#11578 = LINE ( 'NONE', #8161, #6754 ) ;
#11579 = CARTESIAN_POINT ( 'NONE',  ( -52.77438362644100067, 99.17411849586700612, -150.4984795835770228 ) ) ;
#11580 = DIRECTION ( 'NONE',  ( -1.000000000000000000, 0.000000000000000000, 0.000000000000000000 ) ) ;
#11581 = DIRECTION ( 'NONE',  ( 0.000000000000000000, 0.000000000000000000, 1.000000000000000000 ) ) ;
#11582 = FACE_OUTER_BOUND ( 'NONE', #1009, .T. ) ;
#11583 = ORIENTED_EDGE ( 'NONE', *, *, #5085, .F. ) ;
#11584 = DIRECTION ( 'NONE',  ( -0.4226182617406989417, -0.9063077870366502697, 5.175581015019663092E-17 ) ) ;
#11585 = EDGE_CURVE ( 'NONE', #13570, #10232, #9243, .T. ) ;
#11586 = VERTEX_POINT ( 'NONE', #13421 ) ;
#11587 = AXIS2_PLACEMENT_3D ( 'NONE', #12664, #4520, #11421 ) ;
#11588 = ORIENTED_EDGE ( 'NONE', *, *, #13036, .T. ) ;
#11589 = CARTESIAN_POINT ( 'NONE',  ( 17.18164641901421419, -12.00000029085424202, -0.3335879563140091153 ) ) ;
#11590 = ORIENTED_EDGE ( 'NONE', *, *, #197, .F. ) ;
#11591 = EDGE_CURVE ( 'NONE', #4688, #11111, #14572, .T. ) ;
#11592 = CARTESIAN_POINT ( 'NONE',  ( -2.667636957649788698, -1.359375000000169198, -3.248130456407447575 ) ) ;
#11593 = ORIENTED_EDGE ( 'NONE', *, *, #8602, .F. ) ;
#11594 = CARTESIAN_POINT ( 'NONE',  ( 1.929669553967771956, -2.171088562373077124, -3.613309278117248002 ) ) ;
#11595 = DIRECTION ( 'NONE',  ( 0.000000000000000000, 0.000000000000000000, 1.000000000000000000 ) ) ;
#11596 = CARTESIAN_POINT ( 'NONE',  ( -15.50000000000000000, 998.9628421096749662, 22.50000000000000000 ) ) ;
#11597 = AXIS2_PLACEMENT_3D ( 'NONE', #12270, #1642, #11106 ) ;
#11598 = LINE ( 'NONE', #4387, #3296 ) ;
#11599 = VERTEX_POINT ( 'NONE', #12171 ) ;
#11600 = CARTESIAN_POINT ( 'NONE',  ( -52.77438362643999881, 67.53201699523744139, -147.9984795835769944 ) ) ;
#11601 = EDGE_CURVE ( 'NONE', #4413, #10872, #7384, .T. ) ;
#11602 = CARTESIAN_POINT ( 'NONE',  ( 17.16405274069114739, -3.654316742536410256, 0.2664120436859874763 ) ) ;
#11603 = CARTESIAN_POINT ( 'NONE',  ( 6.428219071167060150, 17.69837218853938410, 140.4057819957278355 ) ) ;
#11604 = ORIENTED_EDGE ( 'NONE', *, *, #5728, .T. ) ;
#11605 = EDGE_CURVE ( 'NONE', #5950, #9201, #11945, .T. ) ;
#11606 = VECTOR ( 'NONE', #7203, 1000.000000000000000 ) ;
#11607 = FILL_AREA_STYLE ('',( #4395 ) ) ;
#11608 = CARTESIAN_POINT ( 'NONE',  ( -1.153796164589674156, -0.2881249999999724309, 3.799958344797443210 ) ) ;
#11609 = ORIENTED_EDGE ( 'NONE', *, *, #4221, .T. ) ;
#11610 = CARTESIAN_POINT ( 'NONE',  ( -0.3615547238505233407, -2.319374999999934239, 3.684823279838126187 ) ) ;
#11611 = FACE_OUTER_BOUND ( 'NONE', #15174, .T. ) ;
#11612 = EDGE_CURVE ( 'NONE', #2233, #4222, #8448, .T. ) ;
#11613 = ADVANCED_FACE ( 'NONE', ( #10865 ), #9913, .F. ) ;
#11614 = DIRECTION ( 'NONE',  ( 0.000000000000000000, 0.000000000000000000, -1.000000000000000000 ) ) ;
#11615 = CARTESIAN_POINT ( 'NONE',  ( -46.58670980944423690, 5.000000000000000000, 91.50956111919106206 ) ) ;
#11616 = CIRCLE ( 'NONE', #12372, 10.20000000000000107 ) ;
#11617 = CARTESIAN_POINT ( 'NONE',  ( 0.000000000000000000, 0.000000000000000000, 0.000000000000000000 ) ) ;
#11618 = CARTESIAN_POINT ( 'NONE',  ( -14.25000000000000000, -2.500000000000000000, -23.22168783648699986 ) ) ;
#11619 = DIRECTION ( 'NONE',  ( -1.000000000000000000, 0.000000000000000000, 0.000000000000000000 ) ) ;
#11620 = ADVANCED_FACE ( 'NONE', ( #381 ), #1475, .T. ) ;
#11621 = CARTESIAN_POINT ( 'NONE',  ( 23.25000000000000000, -5.000000000000000000, -27.00000000000000000 ) ) ;
#11622 = ORIENTED_EDGE ( 'NONE', *, *, #13334, .F. ) ;
#11623 = LINE ( 'NONE', #751, #8017 ) ;
#11624 = ORIENTED_EDGE ( 'NONE', *, *, #6325, .F. ) ;
#11625 = EDGE_CURVE ( 'NONE', #2640, #3597, #11270, .T. ) ;
#11626 = ORIENTED_EDGE ( 'NONE', *, *, #10743, .F. ) ;
#11627 = ADVANCED_FACE ( 'NONE', ( #2474 ), #1544, .F. ) ;
#11628 = ORIENTED_EDGE ( 'NONE', *, *, #13708, .F. ) ;
#11629 = VERTEX_POINT ( 'NONE', #10787 ) ;
#11630 = ORIENTED_EDGE ( 'NONE', *, *, #667, .T. ) ;
#11631 = CARTESIAN_POINT ( 'NONE',  ( -3.630878219354529257, -4.452338562373184594, -1.102448361598825644 ) ) ;
#11632 = CARTESIAN_POINT ( 'NONE',  ( -3.563362751979704868, -1.147500000000009734, 1.477520127916053472 ) ) ;
#11633 = CARTESIAN_POINT ( 'NONE',  ( 3.091873775341146491, -2.890625000000027534, 2.538798244104332191 ) ) ;
#11634 = CARTESIAN_POINT ( 'NONE',  ( 24.12375314681476368, -1.228611132858002289E-15, 52.46674979433200292 ) ) ;
#11635 = DIRECTION ( 'NONE',  ( -1.000000000000000000, -2.551930889570659960E-15, 0.000000000000000000 ) ) ;
#11636 = DIRECTION ( 'NONE',  ( 0.000000000000000000, -0.000000000000000000, 1.000000000000000000 ) ) ;
#11637 = CARTESIAN_POINT ( 'NONE',  ( -2.598076211353320453, 2.374999999999993339, 4.500000000000000888 ) ) ;
#11638 = CARTESIAN_POINT ( 'NONE',  ( 0.000000000000000000, 0.000000000000000000, -79.59847958357700293 ) ) ;
#11639 = ORIENTED_EDGE ( 'NONE', *, *, #15221, .F. ) ;
#11640 = CARTESIAN_POINT ( 'NONE',  ( -15.08565937784311295, -0.3156604612129216836, -23.70415600323552852 ) ) ;
#11641 = ORIENTED_EDGE ( 'NONE', *, *, #13896, .T. ) ;
#11642 = ORIENTED_EDGE ( 'NONE', *, *, #11709, .F. ) ;
#11643 = VERTEX_POINT ( 'NONE', #13274 ) ;
#11644 = DIRECTION ( 'NONE',  ( 0.000000000000000000, 0.000000000000000000, 1.000000000000000000 ) ) ;
#11645 = CARTESIAN_POINT ( 'NONE',  ( -16.75000000000000000, -0.2038245569916330158, -23.22168783648699986 ) ) ;
#11646 = DIRECTION ( 'NONE',  ( 1.000000000000000000, 0.000000000000000000, -0.000000000000000000 ) ) ;
#11647 = CARTESIAN_POINT ( 'NONE',  ( -0.2250800285832887659, 2.375126720995723417, -4.499999999999999112 ) ) ;
#11648 = DIRECTION ( 'NONE',  ( 0.000000000000000000, 0.000000000000000000, 1.000000000000000000 ) ) ;
#11649 = B_SPLINE_CURVE_WITH_KNOTS ( 'NONE', 3,
 ( #8829, #7680, #597, #5350 ),
 .UNSPECIFIED., .F., .F.,
 ( 4, 4 ),
 ( 2.309401076754191683E-07, 0.002598307151460989371 ),
 .UNSPECIFIED. ) ;
#11650 = CARTESIAN_POINT ( 'NONE',  ( -91.27438362643999881, 65.17411849586700612, -145.4984795835769660 ) ) ;
#11651 = CARTESIAN_POINT ( 'NONE',  ( 3.897114317029974018, 9.945166405816858860E-15, -2.250000000000001332 ) ) ;
#11652 = CARTESIAN_POINT ( 'NONE',  ( -30.00000000000000000, 0.000000000000000000, 27.00000000000000000 ) ) ;
#11653 = CARTESIAN_POINT ( 'NONE',  ( -65.73898050152220662, 64.78624853950366003, -83.44847958357698303 ) ) ;
#11654 = VERTEX_POINT ( 'NONE', #14341 ) ;
#11655 = CARTESIAN_POINT ( 'NONE',  ( -73.01311196519618818, 67.29799558322736175, -81.84847958357697451 ) ) ;
#11656 = ORIENTED_EDGE ( 'NONE', *, *, #3349, .T. ) ;
#11657 = ORIENTED_EDGE ( 'NONE', *, *, #10413, .T. ) ;
#11658 = DIRECTION ( 'NONE',  ( 0.000000000000000000, 0.000000000000000000, 1.000000000000000000 ) ) ;
#11659 = ORIENTED_EDGE ( 'NONE', *, *, #2992, .T. ) ;
#11660 = CARTESIAN_POINT ( 'NONE',  ( -4.010754789764311212, -1.453125000000109912, -1.215065766439024975 ) ) ;
#11661 = ORIENTED_EDGE ( 'NONE', *, *, #4708, .F. ) ;
#11662 = CARTESIAN_POINT ( 'NONE',  ( -1.540128476469153185, -2.686713562373115760, 3.722025193358375894 ) ) ;
#11663 = DIRECTION ( 'NONE',  ( 0.000000000000000000, 1.000000000000000000, 0.000000000000000000 ) ) ;
#11664 = ADVANCED_FACE ( 'NONE', ( #150 ), #6300, .T. ) ;
#11665 = CARTESIAN_POINT ( 'NONE',  ( -69.77438362644001302, 90.17411849586700612, -58.99847958357700151 ) ) ;
#11666 = VECTOR ( 'NONE', #11154, 1000.000000000000000 ) ;
#11667 = CARTESIAN_POINT ( 'NONE',  ( -50.27438362643999881, 65.17411849586700612, -182.2484795835770228 ) ) ;
#11668 = EDGE_CURVE ( 'NONE', #5825, #5722, #8036, .T. ) ;
#11669 = PRODUCT_DEFINITION_SHAPE ( 'NONE', 'NONE',  #15343 ) ;
#11670 = DIRECTION ( 'NONE',  ( 0.000000000000000000, 0.000000000000000000, -1.000000000000000000 ) ) ;
#11671 = ORIENTED_EDGE ( 'NONE', *, *, #8316, .T. ) ;
#11672 = CARTESIAN_POINT ( 'NONE',  ( 3.315864351079437888, -5.143616724908924631, -1.547231645668555533 ) ) ;
#11673 = DIRECTION ( 'NONE',  ( 0.000000000000000000, 0.000000000000000000, -1.000000000000000000 ) ) ;
#11674 = EDGE_LOOP ( 'NONE', ( #1596, #208 ) ) ;
#11675 = CIRCLE ( 'NONE', #1526, 5.500000000000005329 ) ;
#11676 = PRESENTATION_STYLE_ASSIGNMENT (( #13854 ) ) ;
#11677 = CARTESIAN_POINT ( 'NONE',  ( -2.837724166816209426, -5.390625000000070166, -2.327111198264740999 ) ) ;
#11678 = ORIENTED_EDGE ( 'NONE', *, *, #5194, .T. ) ;
#11679 = EDGE_CURVE ( 'NONE', #11586, #13082, #8528, .T. ) ;
#11680 = CARTESIAN_POINT ( 'NONE',  ( -3.733522804429754149, -2.085000000000140741, 0.001371824453762974898 ) ) ;
#11681 = CARTESIAN_POINT ( 'NONE',  ( -69.77438362644100778, 82.17411849586699191, -79.49847958357700861 ) ) ;
#11682 = EDGE_CURVE ( 'NONE', #14025, #3986, #10767, .T. ) ;
#11683 = AXIS2_PLACEMENT_3D ( 'NONE', #7023, #11749, #7878 ) ;
#11684 = DIRECTION ( 'NONE',  ( -0.9375000000000004441, 0.000000000000000000, -0.3479852726768752902 ) ) ;
#11685 = DIRECTION ( 'NONE',  ( 1.287488025362404182E-15, 1.000000000000000000, 0.000000000000000000 ) ) ;
#11686 = LINE ( 'NONE', #13102, #12611 ) ;
#11687 = DIRECTION ( 'NONE',  ( 0.000000000000000000, 0.000000000000000000, -1.000000000000000000 ) ) ;
#11688 = CARTESIAN_POINT ( 'NONE',  ( -12.81835358098578403, -12.60000029085423812, -8.183940086454239093 ) ) ;
#11689 = CIRCLE ( 'NONE', #8715, 3.300000002979700753 ) ;
#11690 = APPLICATION_CONTEXT ( 'automotive_design' ) ;
#11691 = CARTESIAN_POINT ( 'NONE',  ( 0.000000000000000000, 0.000000000000000000, 6.000000000000000000 ) ) ;
#11692 = ORIENTED_EDGE ( 'NONE', *, *, #5660, .T. ) ;
#11693 = DIRECTION ( 'NONE',  ( 0.000000000000000000, 1.000000000000000000, 0.000000000000000000 ) ) ;
#11694 = EDGE_LOOP ( 'NONE', ( #9400, #1108, #69, #648 ) ) ;
#11695 = AXIS2_PLACEMENT_3D ( 'NONE', #13608, #7714, #12439 ) ;
#11696 = ADVANCED_FACE ( 'NONE', ( #8678 ), #3953, .T. ) ;
#11697 = ORIENTED_EDGE ( 'NONE', *, *, #5951, .T. ) ;
#11698 = CARTESIAN_POINT ( 'NONE',  ( -0.9755776780686776783, -4.881874999999863185, -3.218989981404325462 ) ) ;
#11699 = EDGE_LOOP ( 'NONE', ( #13175, #15327, #8945, #15139 ) ) ;
#11700 = ORIENTED_EDGE ( 'NONE', *, *, #4204, .T. ) ;
#11701 = ORIENTED_EDGE ( 'NONE', *, *, #13815, .T. ) ;
#11702 = CARTESIAN_POINT ( 'NONE',  ( 2.889335172541571684, -4.889838562373118869, 2.369440177208199660 ) ) ;
#11703 = VECTOR ( 'NONE', #3664, 1000.000000000000000 ) ;
#11704 = FACE_OUTER_BOUND ( 'NONE', #11313, .T. ) ;
#11705 = ADVANCED_FACE ( 'NONE', ( #13500, #13578 ), #533, .T. ) ;
#11706 = DIRECTION ( 'NONE',  ( 0.000000000000000000, 0.000000000000000000, 1.000000000000000000 ) ) ;
#11707 = CARTESIAN_POINT ( 'NONE',  ( -101.2743836264399988, 111.1741184958670061, -79.49847958357700861 ) ) ;
#11708 = CYLINDRICAL_SURFACE ( 'NONE', #12074, 9.999999999999994671 ) ;
#11709 = EDGE_CURVE ( 'NONE', #188, #7936, #6449, .T. ) ;
#11710 = MECHANICAL_DESIGN_GEOMETRIC_PRESENTATION_REPRESENTATION (  '', ( #4527 ), #12459 ) ;
#11711 = ADVANCED_FACE ( 'NONE', ( #9057 ), #12486, .F. ) ;
#11712 = CARTESIAN_POINT ( 'NONE',  ( -56.85838362644099675, 99.17411849586700612, -147.9984795835769944 ) ) ;
#11713 = B_SPLINE_CURVE_WITH_KNOTS ( 'NONE', 3,
 ( #5584, #10288, #1523, #47, #13171, #13251, #9739, #3931, #7282, #9821, #4791, #2530, #6278, #12006 ),
 .UNSPECIFIED., .F., .F.,
 ( 4, 2, 2, 2, 2, 2, 4 ),
 ( 0.002345953150261289536, 0.002784084228693953569, 0.003222215307126618036, 0.004098477463991946970, 0.004536608542424611437, 0.004974739620857275037, 0.005851001777722601369 ),
 .UNSPECIFIED. ) ;
#11714 = DIRECTION ( 'NONE',  ( 0.000000000000000000, -1.000000000000000000, 0.000000000000000000 ) ) ;
#11715 = CARTESIAN_POINT ( 'NONE',  ( 14.25000000000000000, -2.500000000000000000, -23.22168783648699986 ) ) ;
#11716 = CARTESIAN_POINT ( 'NONE',  ( 3.009749400183384882, -4.506874999999939568, 1.609730366092098075 ) ) ;
#11717 = CARTESIAN_POINT ( 'NONE',  ( -4.435020996998820131, -12.00000029085427045, 69.03723529703216855 ) ) ;
#11718 = EDGE_LOOP ( 'NONE', ( #11436, #2493, #3209, #2696 ) ) ;
#11719 = DIRECTION ( 'NONE',  ( 0.000000000000000000, 0.000000000000000000, 1.000000000000000000 ) ) ;
#11720 = AXIS2_PLACEMENT_3D ( 'NONE', #3407, #14036, #14183 ) ;
#11721 = ORIENTED_EDGE ( 'NONE', *, *, #10464, .T. ) ;
#11722 = EDGE_CURVE ( 'NONE', #7228, #8110, #8834, .T. ) ;
#11723 = ORIENTED_EDGE ( 'NONE', *, *, #8917, .F. ) ;
#11724 = ORIENTED_EDGE ( 'NONE', *, *, #713, .F. ) ;
#11725 = VECTOR ( 'NONE', #2424, 1000.000000000000000 ) ;
#11726 = CARTESIAN_POINT ( 'NONE',  ( 35.35543536254876074, -3.618985300545107364, 6.000000000000000000 ) ) ;
#11727 = CARTESIAN_POINT ( 'NONE',  ( -0.9979582191391829227, -4.288125000000008846, 3.294238300096191452 ) ) ;
#11728 = EDGE_CURVE ( 'NONE', #10442, #777, #11160, .T. ) ;
#11729 = CARTESIAN_POINT ( 'NONE',  ( -54.81638362644000040, 63.99516924618178848, -150.4984795835770228 ) ) ;
#11730 = CARTESIAN_POINT ( 'NONE',  ( 3.721607743032638638, -5.000000000000047073, 0.0009661164014421728431 ) ) ;
#11731 = DIRECTION ( 'NONE',  ( 0.000000000000000000, 0.000000000000000000, -1.000000000000000000 ) ) ;
#11732 = CONICAL_SURFACE ( 'NONE', #13468, 2.042000000000002036, 1.047197551196596965 ) ;
#11733 = CARTESIAN_POINT ( 'NONE',  ( -69.77438362643999881, 89.17411849586052597, -43.99847958364157563 ) ) ;
#11734 = FACE_OUTER_BOUND ( 'NONE', #870, .T. ) ;
#11735 = CARTESIAN_POINT ( 'NONE',  ( 1.603389813606017622, -12.00000029085424735, 0.01788390626212849749 ) ) ;
#11736 = CARTESIAN_POINT ( 'NONE',  ( 11.02010870769206541, -85.69524470659703752, 70.09311034953161368 ) ) ;
#11737 = FACE_BOUND ( 'NONE', #3596, .T. ) ;
#11738 = AXIS2_PLACEMENT_3D ( 'NONE', #8068, #8383, #13124 ) ;
#11739 = ORIENTED_EDGE ( 'NONE', *, *, #10634, .F. ) ;
#11740 = DIRECTION ( 'NONE',  ( 0.000000000000000000, -1.000000000000000000, 0.000000000000000000 ) ) ;
#11741 = EDGE_LOOP ( 'NONE', ( #9404, #14912, #13635, #3386 ) ) ;
#11742 = VERTEX_POINT ( 'NONE', #6601 ) ;
#11743 = CIRCLE ( 'NONE', #4815, 3.000000000000002665 ) ;
#11744 = ORIENTED_EDGE ( 'NONE', *, *, #11955, .T. ) ;
#11745 = AXIS2_PLACEMENT_3D ( 'NONE', #12257, #12488, #8909 ) ;
#11746 = CARTESIAN_POINT ( 'NONE',  ( -69.77438362644001302, 82.17411849586700612, -81.84847958357698872 ) ) ;
#11747 = VERTEX_POINT ( 'NONE', #5586 ) ;
#11748 = CARTESIAN_POINT ( 'NONE',  ( 3.069693586880715142, -3.108588562373168163, -2.521103932842495343 ) ) ;
#11749 = DIRECTION ( 'NONE',  ( 0.000000000000000000, 0.000000000000000000, -1.000000000000000000 ) ) ;
#11750 = DIRECTION ( 'NONE',  ( -1.000000000000000000, 0.000000000000000000, 0.000000000000000000 ) ) ;
#11751 = CARTESIAN_POINT ( 'NONE',  ( 5.196152422706626695, 1.678847577293385296, -1.115338501812287204E-15 ) ) ;
#11752 = AXIS2_PLACEMENT_3D ( 'NONE', #12416, #9765, #14422 ) ;
#11753 = VECTOR ( 'NONE', #7052, 1000.000000000000000 ) ;
#11754 = CARTESIAN_POINT ( 'NONE',  ( 57.41329019055577021, 5.000000000000001776, 129.5095611191910621 ) ) ;
#11755 = ORIENTED_EDGE ( 'NONE', *, *, #12184, .T. ) ;
#11756 = DIRECTION ( 'NONE',  ( 0.000000000000000000, 0.000000000000000000, -1.000000000000000000 ) ) ;
#11757 = CARTESIAN_POINT ( 'NONE',  ( -54.81638362644000040, 63.99516924618178848, -147.9984795835769944 ) ) ;
#11758 = VERTEX_POINT ( 'NONE', #6675 ) ;
#11759 = SURFACE_STYLE_FILL_AREA ( #14463 ) ;
#11760 = CARTESIAN_POINT ( 'NONE',  ( 3.915012698312750228, -0.5693749999999865308, 0.3866328316385075348 ) ) ;
#11761 = VERTEX_POINT ( 'NONE', #2943 ) ;
#11762 = ADVANCED_FACE ( 'NONE', ( #7684 ), #3165, .F. ) ;
#11763 = AXIS2_PLACEMENT_3D ( 'NONE', #2374, #7127, #5019 ) ;
#11764 = CARTESIAN_POINT ( 'NONE',  ( -2.084927739720960016, -1.928749999999817888, -3.122072247380865306 ) ) ;
#11765 = PLANE ( 'NONE',  #5232 ) ;
#11766 = CARTESIAN_POINT ( 'NONE',  ( 22.58164641901421632, -12.60000029085423812, -8.183940086454239093 ) ) ;
#11767 = DIRECTION ( 'NONE',  ( 0.000000000000000000, 0.000000000000000000, -1.000000000000000000 ) ) ;
#11768 = FACE_OUTER_BOUND ( 'NONE', #11470, .T. ) ;
#11769 = CARTESIAN_POINT ( 'NONE',  ( -66.62325245518700001, 94.57411849586699759, -93.49847958357699440 ) ) ;
#11770 = CARTESIAN_POINT ( 'NONE',  ( -88.81638362644000040, 63.99516924618178848, -147.9984795835769944 ) ) ;
#11771 = CIRCLE ( 'NONE', #9536, 0.8000000000000113687 ) ;
#11772 = EDGE_LOOP ( 'NONE', ( #7304, #8680, #13336 ) ) ;
#11773 = AXIS2_PLACEMENT_3D ( 'NONE', #13743, #4271, #3189 ) ;
#11774 = EDGE_CURVE ( 'NONE', #5737, #2678, #9283, .T. ) ;
#11775 = ORIENTED_EDGE ( 'NONE', *, *, #1470, .F. ) ;
#11776 = EDGE_LOOP ( 'NONE', ( #1008, #11471, #4795, #7076, #5587 ) ) ;
#11777 = CARTESIAN_POINT ( 'NONE',  ( -2.211816241884709822, -3.944375000000018172, -2.696513105594181336 ) ) ;
#11778 = ORIENTED_EDGE ( 'NONE', *, *, #13630, .F. ) ;
#11779 = ORIENTED_EDGE ( 'NONE', *, *, #5470, .F. ) ;
#11780 = ADVANCED_FACE ( 'NONE', ( #7612 ), #3015, .F. ) ;
#11781 = ORIENTED_EDGE ( 'NONE', *, *, #2772, .F. ) ;
#11782 = CARTESIAN_POINT ( 'NONE',  ( 3.702328265034185772, -5.014838562373222786, -0.3636771760147958776 ) ) ;
#11783 = AXIS2_PLACEMENT_3D ( 'NONE', #10640, #9470, #9547 ) ;
#11784 = LINE ( 'NONE', #10688, #6330 ) ;
#11785 = AXIS2_PLACEMENT_3D ( 'NONE', #13540, #14601, #2905 ) ;
#11786 = AXIS2_PLACEMENT_3D ( 'NONE', #9755, #12250, #11090 ) ;
#11787 = PLANE ( 'NONE',  #10316 ) ;
#11788 = DIRECTION ( 'NONE',  ( 0.000000000000000000, 0.000000000000000000, 1.000000000000000000 ) ) ;
#11789 = DIRECTION ( 'NONE',  ( -0.000000000000000000, -0.000000000000000000, 1.000000000000000000 ) ) ;
#11790 =( REPRESENTATION_RELATIONSHIP ('NONE','NONE', #12357, #6613 ) REPRESENTATION_RELATIONSHIP_WITH_TRANSFORMATION ( #3845 )SHAPE_REPRESENTATION_RELATIONSHIP( ) );
#11791 = DIRECTION ( 'NONE',  ( 0.5000000000000003331, 0.8660254037844384856, 0.000000000000000000 ) ) ;
#11792 = CARTESIAN_POINT ( 'NONE',  ( -52.77438362644000591, 99.17411849586700612, -86.49847958357699440 ) ) ;
#11793 = DIRECTION ( 'NONE',  ( 1.000000000000000000, 0.000000000000000000, 0.000000000000000000 ) ) ;
#11794 = CARTESIAN_POINT ( 'NONE',  ( -2.189584623831577037, -4.225624999999936016, 2.666627758504775958 ) ) ;
#11795 = DIRECTION ( 'NONE',  ( 0.000000000000000000, 0.000000000000000000, -1.000000000000000000 ) ) ;
#11796 = ORIENTED_EDGE ( 'NONE', *, *, #7538, .T. ) ;
#11797 = FACE_OUTER_BOUND ( 'NONE', #7765, .T. ) ;
#11798 = AXIS2_PLACEMENT_3D ( 'NONE', #5608, #4499, #12804 ) ;
#11799 = EDGE_CURVE ( 'NONE', #15133, #2626, #11312, .T. ) ;
#11800 = ORIENTED_EDGE ( 'NONE', *, *, #11010, .T. ) ;
#11801 = VECTOR ( 'NONE', #8162, 1000.000000000000000 ) ;
#11802 = EDGE_LOOP ( 'NONE', ( #13344, #5764 ) ) ;
#11803 = EDGE_LOOP ( 'NONE', ( #3725, #4468, #12009, #3041 ) ) ;
#11804 = AXIS2_PLACEMENT_3D ( 'NONE', #14551, #13402, #360 ) ;
#11805 = EDGE_CURVE ( 'NONE', #5361, #3573, #1780, .T. ) ;
#11806 = CARTESIAN_POINT ( 'NONE',  ( -2.773226354234704427, -3.194375000000006182, 2.274732928208734961 ) ) ;
#11807 = LINE ( 'NONE', #11729, #1650 ) ;
#11808 = AXIS2_PLACEMENT_3D ( 'NONE', #9180, #8029, #15149 ) ;
#11809 = LINE ( 'NONE', #1175, #10963 ) ;
#11810 = CARTESIAN_POINT ( 'NONE',  ( -69.77438362644001302, 81.46011849586699327, -81.84847958357697451 ) ) ;
#11811 = DIRECTION ( 'NONE',  ( 1.000000000000000000, -0.000000000000000000, 0.000000000000000000 ) ) ;
#11812 = EDGE_CURVE ( 'NONE', #13217, #12323, #681, .T. ) ;
#11813 = CARTESIAN_POINT ( 'NONE',  ( -53.77438362644000591, 82.17411849586700612, -112.9984795835769944 ) ) ;
#11814 = CARTESIAN_POINT ( 'NONE',  ( -4.296774773080532128, -0.4990699899015805241, -0.003879984233104640575 ) ) ;
#11815 = CARTESIAN_POINT ( 'NONE',  ( -69.77438362644001302, 82.17411849586700612, -150.4984795835769944 ) ) ;
#11816 = DIRECTION ( 'NONE',  ( 0.000000000000000000, 0.000000000000000000, 1.000000000000000000 ) ) ;
#11817 = VERTEX_POINT ( 'NONE', #4252 ) ;
#11818 = DIRECTION ( 'NONE',  ( 0.8660254037844387076, 0.4999999999999998890, 0.000000000000000000 ) ) ;
#11819 = ADVANCED_FACE ( 'NONE', ( #13722 ), #14795, .F. ) ;
#11820 = ORIENTED_EDGE ( 'NONE', *, *, #8012, .F. ) ;
#11821 = EDGE_LOOP ( 'NONE', ( #7173, #8516, #8662, #12947 ) ) ;
#11822 = AXIS2_PLACEMENT_3D ( 'NONE', #5569, #10047, #1123 ) ;
#11823 = ADVANCED_FACE ( 'NONE', ( #5507 ), #12563, .F. ) ;
#11824 = AXIS2_PLACEMENT_3D ( 'NONE', #8521, #13573, #9669 ) ;
#11825 = CARTESIAN_POINT ( 'NONE',  ( -3.065271248674581006, -0.3749999999999933942, -3.063065156281021384 ) ) ;
#11826 = EDGE_CURVE ( 'NONE', #9509, #6831, #12680, .T. ) ;
#11827 = ORIENTED_EDGE ( 'NONE', *, *, #13892, .F. ) ;
#11828 = CARTESIAN_POINT ( 'NONE',  ( -3.040116134197859754, -0.6242135623732079086, 3.042307828174728446 ) ) ;
#11829 = DIRECTION ( 'NONE',  ( -1.000000000000000000, 1.734723475976808672E-15, 5.828670879282076886E-13 ) ) ;
#11830 = CARTESIAN_POINT ( 'NONE',  ( 15.50000000000000000, 998.9628421096749662, -22.50000000000000000 ) ) ;
#11831 = CARTESIAN_POINT ( 'NONE',  ( 14.24999999999999822, -0.3152037684892576297, 22.74589050208021845 ) ) ;
#11832 = AXIS2_PLACEMENT_3D ( 'NONE', #13682, #6560, #8941 ) ;
#11833 = DIRECTION ( 'NONE',  ( 0.000000000000000000, 0.000000000000000000, -1.000000000000000000 ) ) ;
#11834 = EDGE_LOOP ( 'NONE', ( #4953, #11876, #13128 ) ) ;
#11835 = LINE ( 'NONE', #11600, #4143 ) ;
#11836 = CARTESIAN_POINT ( 'NONE',  ( -96.77438362643999881, 59.67411849586700612, -15.85886927678779834 ) ) ;
#11837 = APPLICATION_PROTOCOL_DEFINITION ( 'draft international standard', 'automotive_design', 1998, #1975 ) ;
#11838 = VERTEX_POINT ( 'NONE', #11770 ) ;
#11839 =( LENGTH_UNIT ( ) NAMED_UNIT ( * ) SI_UNIT ( .MILLI., .METRE. ) );
#11840 = CARTESIAN_POINT ( 'NONE',  ( -3.920035875790600421, -3.499999999999977796, -0.001028343392498549860 ) ) ;
#11841 = ORIENTED_EDGE ( 'NONE', *, *, #331, .F. ) ;
#11842 = VECTOR ( 'NONE', #14358, 1000.000000000000000 ) ;
#11843 = PLANE ( 'NONE',  #13666 ) ;
#11844 = CARTESIAN_POINT ( 'NONE',  ( -3.238071519113512320, -5.298747598780473744, 1.157691333774819364 ) ) ;
#11845 = FACE_OUTER_BOUND ( 'NONE', #8610, .T. ) ;
#11846 = LINE ( 'NONE', #2219, #9757 ) ;
#11847 = CARTESIAN_POINT ( 'NONE',  ( -88.81638362644100937, 97.99516924618178848, -147.9984795835769944 ) ) ;
#11848 = DIRECTION ( 'NONE',  ( 0.000000000000000000, -0.000000000000000000, 1.000000000000000000 ) ) ;
#11849 = DIRECTION ( 'NONE',  ( 0.000000000000000000, 1.000000000000000000, 0.000000000000000000 ) ) ;
#11850 = CARTESIAN_POINT ( 'NONE',  ( -62.02799568714584666, 0.000000000000000000, -79.59847958357700293 ) ) ;
#11851 = CIRCLE ( 'NONE', #5175, 2.042000000000002036 ) ;
#11852 = EDGE_LOOP ( 'NONE', ( #12572, #10824, #6827, #1456 ) ) ;
#11853 = DIRECTION ( 'NONE',  ( 1.000000000000000000, 0.000000000000000000, 0.000000000000000000 ) ) ;
#11854 =( NAMED_UNIT ( * ) PLANE_ANGLE_UNIT ( ) SI_UNIT ( $, .RADIAN. ) );
#11855 = ORIENTED_EDGE ( 'NONE', *, *, #5654, .T. ) ;
#11856 = FACE_BOUND ( 'NONE', #11384, .T. ) ;
#11857 = CARTESIAN_POINT ( 'NONE',  ( 2.315514200798128197, -2.725624999999891607, -2.819975302942780981 ) ) ;
#11858 = ORIENTED_EDGE ( 'NONE', *, *, #3952, .F. ) ;
#11859 = VERTEX_POINT ( 'NONE', #4717 ) ;
#11860 = VERTEX_POINT ( 'NONE', #3232 ) ;
#11861 = CARTESIAN_POINT ( 'NONE',  ( -1.458314181602024417, -4.311713562372998965, -3.523281483662707547 ) ) ;
#11862 = DIRECTION ( 'NONE',  ( 0.000000000000000000, 0.000000000000000000, -1.000000000000000000 ) ) ;
#11863 = CIRCLE ( 'NONE', #5429, 8.124999999999992895 ) ;
#11864 = FACE_OUTER_BOUND ( 'NONE', #4780, .T. ) ;
#11865 = DIRECTION ( 'NONE',  ( 0.000000000000000000, 0.000000000000000000, -1.000000000000000000 ) ) ;
#11866 = EDGE_CURVE ( 'NONE', #11017, #59, #3509, .T. ) ;
#11867 = DIRECTION ( 'NONE',  ( 0.000000000000000000, 0.000000000000000000, -1.000000000000000000 ) ) ;
#11868 = LINE ( 'NONE', #65, #1938 ) ;
#11869 = DIRECTION ( 'NONE',  ( 0.000000000000000000, 0.000000000000000000, 1.000000000000000000 ) ) ;
#11870 = FACE_BOUND ( 'NONE', #9594, .T. ) ;
#11871 = EDGE_CURVE ( 'NONE', #9154, #13931, #981, .T. ) ;
#11872 = CARTESIAN_POINT ( 'NONE',  ( -3.319861881881159160, -3.147500000000079456, 1.374129751973758307 ) ) ;
#11873 = DIRECTION ( 'NONE',  ( -0.000000000000000000, 4.336808689942017736E-16, -1.000000000000000000 ) ) ;
#11874 = ORIENTED_EDGE ( 'NONE', *, *, #10473, .T. ) ;
#11875 = DIRECTION ( 'NONE',  ( 0.000000000000000000, 0.000000000000000000, -1.000000000000000000 ) ) ;
#11876 = ORIENTED_EDGE ( 'NONE', *, *, #8487, .T. ) ;
#11877 = ORIENTED_EDGE ( 'NONE', *, *, #5559, .T. ) ;
#11878 = ORIENTED_EDGE ( 'NONE', *, *, #526, .T. ) ;
#11879 = CARTESIAN_POINT ( 'NONE',  ( -86.77438362644100778, 99.17411849586700612, -149.9984795835770228 ) ) ;
#11880 = CARTESIAN_POINT ( 'NONE',  ( 0.3668491701747067513, -4.765624999999817923, 3.734637934618871391 ) ) ;
#11881 = CARTESIAN_POINT ( 'NONE',  ( -0.9013897962190543511, 2.290928418201631622, -4.499999999999999112 ) ) ;
#11882 = ADVANCED_FACE ( 'NONE', ( #5668 ), #5976, .F. ) ;
#11883 = CARTESIAN_POINT ( 'NONE',  ( -80.52077156573417938, 60.67411849586702743, -152.4984795835769944 ) ) ;
#11884 = PRODUCT_DEFINITION_FORMATION_WITH_SPECIFIED_SOURCE ( 'ANY', '', #5345, .NOT_KNOWN. ) ;
#11885 = CARTESIAN_POINT ( 'NONE',  ( -86.77438362644001302, 99.17411849586700612, -86.49847958357699440 ) ) ;
#11886 = DIRECTION ( 'NONE',  ( 0.000000000000000000, -1.000000000000000000, -4.336808689942017736E-16 ) ) ;
#11887 = PLANE ( 'NONE',  #13499 ) ;
#11888 = DIRECTION ( 'NONE',  ( -0.000000000000000000, -0.000000000000000000, -1.000000000000000000 ) ) ;
#11889 = B_SPLINE_CURVE_WITH_KNOTS ( 'NONE', 3,
 ( #10115, #12540, #1904, #11831, #9408, #26 ),
 .UNSPECIFIED., .F., .F.,
 ( 4, 2, 4 ),
 ( 1.820537833122031657, 2.555393473688636341, 3.290249114255240581 ),
 .UNSPECIFIED. ) ;
#11890 = CARTESIAN_POINT ( 'NONE',  ( -52.77438362643999881, 67.53201699523744139, -150.4984795835770228 ) ) ;
#11891 = ORIENTED_EDGE ( 'NONE', *, *, #4046, .T. ) ;
#11892 = DIRECTION ( 'NONE',  ( -0.9961946980917453232, 7.200509705930738460E-17, -0.08715574274766157981 ) ) ;
#11893 = ORIENTED_EDGE ( 'NONE', *, *, #7660, .T. ) ;
#11894 = ORIENTED_EDGE ( 'NONE', *, *, #8652, .F. ) ;
#11895 = VERTEX_POINT ( 'NONE', #12784 ) ;
#11896 = DIRECTION ( 'NONE',  ( 0.000000000000000000, 0.000000000000000000, 1.000000000000000000 ) ) ;
#11897 = EDGE_CURVE ( 'NONE', #8008, #11322, #9445, .T. ) ;
#11898 = DIRECTION ( 'NONE',  ( 0.000000000000000000, 0.000000000000000000, 1.000000000000000000 ) ) ;
#11899 = ORIENTED_EDGE ( 'NONE', *, *, #151, .F. ) ;
#11900 = EDGE_CURVE ( 'NONE', #14122, #11302, #4557, .T. ) ;
#11901 = CARTESIAN_POINT ( 'NONE',  ( -0.4121457528836308115, -1.264838562373080677, -4.196025130973226602 ) ) ;
#11902 = DIRECTION ( 'NONE',  ( 0.000000000000000000, 0.000000000000000000, 1.000000000000000000 ) ) ;
#11903 = EDGE_CURVE ( 'NONE', #8783, #3610, #10365, .T. ) ;
#11904 = FACE_OUTER_BOUND ( 'NONE', #1850, .T. ) ;
#11905 = LINE ( 'NONE', #11667, #15175 ) ;
#11906 = ADVANCED_FACE ( 'NONE', ( #6823 ), #1217, .F. ) ;
#11907 = FACE_OUTER_BOUND ( 'NONE', #7194, .T. ) ;
#11908 = ADVANCED_FACE ( 'NONE', ( #9197 ), #12701, .F. ) ;
#11909 = ORIENTED_EDGE ( 'NONE', *, *, #2499, .T. ) ;
#11910 = B_SPLINE_CURVE_WITH_KNOTS ( 'NONE', 3,
 ( #4205, #1871, #6695, #13599, #770, #13745 ),
 .UNSPECIFIED., .F., .F.,
 ( 4, 2, 4 ),
 ( 1.820537833122030991, 2.555393473688635453, 3.290249114255240137 ),
 .UNSPECIFIED. ) ;
#11911 = LINE ( 'NONE', #15310, #10825 ) ;
#11912 = DIRECTION ( 'NONE',  ( -1.000000000000000000, -1.783664229908549233E-15, 0.000000000000000000 ) ) ;
#11913 = VERTEX_POINT ( 'NONE', #11621 ) ;
#11914 = DIRECTION ( 'NONE',  ( -0.000000000000000000, -0.000000000000000000, 1.000000000000000000 ) ) ;
#11915 = EDGE_CURVE ( 'NONE', #3573, #1497, #287, .T. ) ;
#11916 = CARTESIAN_POINT ( 'NONE',  ( 1.127871658241229147, -3.796875000000003553, 3.713209756639876069 ) ) ;
#11917 = ORIENTED_EDGE ( 'NONE', *, *, #2223, .F. ) ;
#11918 = VECTOR ( 'NONE', #4636, 1000.000000000000000 ) ;
#11919 = CARTESIAN_POINT ( 'NONE',  ( 2.769370807496521980, -0.7100000000000333822, -2.767918543042355850 ) ) ;
#11920 = ADVANCED_FACE ( 'NONE', ( #2380 ), #13938, .T. ) ;
#11921 = DIRECTION ( 'NONE',  ( 0.000000000000000000, 0.000000000000000000, 1.000000000000000000 ) ) ;
#11922 = CARTESIAN_POINT ( 'NONE',  ( 57.41329019055577021, 0.000000000000000000, 131.2954986191910791 ) ) ;
#11923 = CIRCLE ( 'NONE', #2745, 3.499999999999999556 ) ;
#11924 = DIRECTION ( 'NONE',  ( 0.000000000000000000, 0.000000000000000000, -1.000000000000000000 ) ) ;
#11925 = DIRECTION ( 'NONE',  ( 0.000000000000000000, 0.000000000000000000, -1.000000000000000000 ) ) ;
#11926 = PLANE ( 'NONE',  #14019 ) ;
#11927 = CIRCLE ( 'NONE', #3246, 0.5999999999999998668 ) ;
#11928 = VERTEX_POINT ( 'NONE', #50 ) ;
#11929 = CARTESIAN_POINT ( 'NONE',  ( -87.79538362644099436, 97.40569462133919387, -147.9984795835769944 ) ) ;
#11930 = VERTEX_POINT ( 'NONE', #7131 ) ;
#11931 = DIRECTION ( 'NONE',  ( 0.000000000000000000, -1.000000000000000000, 0.000000000000000000 ) ) ;
#11932 = CARTESIAN_POINT ( 'NONE',  ( 3.109021928378527644, -3.663124999999927578, -1.660781358203028413 ) ) ;
#11933 = ORIENTED_EDGE ( 'NONE', *, *, #8119, .T. ) ;
#11934 = ORIENTED_EDGE ( 'NONE', *, *, #10099, .F. ) ;
#11935 = VERTEX_POINT ( 'NONE', #3313 ) ;
#11936 = AXIS2_PLACEMENT_3D ( 'NONE', #2129, #2274, #3290 ) ;
#11937 = DIRECTION ( 'NONE',  ( 1.287488025362404182E-15, 1.000000000000000000, 0.000000000000000000 ) ) ;
#11938 = FACE_OUTER_BOUND ( 'NONE', #4253, .T. ) ;
#11939 = VECTOR ( 'NONE', #5902, 1000.000000000000000 ) ;
#11940 = B_SPLINE_CURVE_WITH_KNOTS ( 'NONE', 3,
 ( #7679, #3790, #11086, #14402, #12165, #13265, #14567, #2775, #458, #8603, #11231, #12403, #6220, #7528, #1765, #9981, #2632, #286, #1616, #12100, #14486, #5196, #13347, #4100, #9907, #14633, #2705, #7449, #373, #8747 ),
 .UNSPECIFIED., .F., .F.,
 ( 4, 2, 2, 2, 2, 2, 2, 2, 2, 2, 2, 2, 2, 2, 4 ),
 ( 0.007091189036500678694, 0.007645091323452510995, 0.008198993610404343296, 0.008752895897356175597, 0.009306798184308006164, 0.009860700471259838465, 0.01041460275821166903, 0.01096850504516350133, 0.01152240733211533363, 0.01207630961906716247, 0.01263021190601899477, 0.01373801647992265763, 0.01484582105382632224, 0.01539972334077815454, 0.01595362562772998510 ),
 .UNSPECIFIED. ) ;
#11941 = DIRECTION ( 'NONE',  ( 0.000000000000000000, 0.000000000000000000, 1.000000000000000000 ) ) ;
#11942 = CARTESIAN_POINT ( 'NONE',  ( -54.81638362644000040, 65.17411849586700612, -147.9984795835769944 ) ) ;
#11943 = CARTESIAN_POINT ( 'NONE',  ( -65.78565528768382364, 67.29799558322736175, -83.44847958357698303 ) ) ;
#11944 = CARTESIAN_POINT ( 'NONE',  ( 1.033118776976089670, -3.381875000000070131, 3.408891928937246796 ) ) ;
#11945 = LINE ( 'NONE', #5201, #6549 ) ;
#11946 = CIRCLE ( 'NONE', #13440, 5.499999999999998224 ) ;
#11947 = ORIENTED_EDGE ( 'NONE', *, *, #13519, .T. ) ;
#11948 = FACE_OUTER_BOUND ( 'NONE', #13584, .T. ) ;
#11949 = ORIENTED_EDGE ( 'NONE', *, *, #4156, .F. ) ;
#11950 = AXIS2_PLACEMENT_3D ( 'NONE', #11726, #2332, #7229 ) ;
#11951 = ORIENTED_EDGE ( 'NONE', *, *, #322, .F. ) ;
#11952 = ORIENTED_EDGE ( 'NONE', *, *, #5456, .T. ) ;
#11953 = DIRECTION ( 'NONE',  ( 0.000000000000000000, 0.000000000000000000, -1.000000000000000000 ) ) ;
#11954 = CARTESIAN_POINT ( 'NONE',  ( 3.535094671665813593, -3.584999999999991083, -0.001309597400350119394 ) ) ;
#11955 = EDGE_CURVE ( 'NONE', #4275, #5866, #3468, .T. ) ;
#11956 = STYLED_ITEM ( 'NONE', ( #14861 ), #10636 ) ;
#11957 = SURFACE_STYLE_USAGE ( .BOTH. , #8079 ) ;
#11958 = DIRECTION ( 'NONE',  ( -0.7071067811865524577, 0.000000000000000000, 0.7071067811865425767 ) ) ;
#11959 = DIRECTION ( 'NONE',  ( 1.000000000000000000, 0.000000000000000000, 0.000000000000000000 ) ) ;
#11960 = DIRECTION ( 'NONE',  ( 0.000000000000000000, 0.7071067811865510144, 0.7071067811865441310 ) ) ;
#11961 = DIRECTION ( 'NONE',  ( 0.000000000000000000, -0.1666666666666656582, 0.9860132971832695770 ) ) ;
#11962 = CARTESIAN_POINT ( 'NONE',  ( -53.79538362643999960, 63.40569462133918677, -147.9984795835769944 ) ) ;
#11963 = CARTESIAN_POINT ( 'NONE',  ( -15.50000000000000000, -1.037157890325000054, -22.50000000000000000 ) ) ;
#11964 = AXIS2_PLACEMENT_3D ( 'NONE', #11479, #847, #9374 ) ;
#11965 = DIRECTION ( 'NONE',  ( 2.551930889570659960E-15, -1.000000000000000000, -0.000000000000000000 ) ) ;
#11966 = LINE ( 'NONE', #1332, #6045 ) ;
#11967 = ORIENTED_EDGE ( 'NONE', *, *, #14653, .F. ) ;
#11968 = DIRECTION ( 'NONE',  ( 1.000000000000000000, -0.000000000000000000, 0.000000000000000000 ) ) ;
#11969 = ORIENTED_EDGE ( 'NONE', *, *, #14095, .F. ) ;
#11970 = VECTOR ( 'NONE', #13, 1000.000000000000114 ) ;
#11971 = ORIENTED_EDGE ( 'NONE', *, *, #4136, .T. ) ;
#11972 = CARTESIAN_POINT ( 'NONE',  ( -16.75000000000000000, -2.500000000000000000, 21.77831216351300014 ) ) ;
#11973 = B_SPLINE_CURVE_WITH_KNOTS ( 'NONE', 3,
 ( #8542, #4044, #14585, #3893 ),
 .UNSPECIFIED., .F., .F.,
 ( 4, 4 ),
 ( 0.01181595095932581191, 0.01442070979368249156 ),
 .UNSPECIFIED. ) ;
#11974 = EDGE_CURVE ( 'NONE', #12114, #2501, #2224, .T. ) ;
#11975 = CARTESIAN_POINT ( 'NONE',  ( 3.088407327495258148, -0.1250000000000329736, -3.086755025163618882 ) ) ;
#11976 = ORIENTED_EDGE ( 'NONE', *, *, #15220, .F. ) ;
#11977 = VECTOR ( 'NONE', #885, 1000.000000000000000 ) ;
#11978 = CARTESIAN_POINT ( 'NONE',  ( 1.637824775874881178, -0.8117135623732008032, 3.950029390179780719 ) ) ;
#11979 = EDGE_CURVE ( 'NONE', #10427, #12362, #1056, .T. ) ;
#11980 = VECTOR ( 'NONE', #11875, 1000.000000000000000 ) ;
#11981 = CARTESIAN_POINT ( 'NONE',  ( -15.70313394609756585, -0.2715358723600081459, 21.17390376548697262 ) ) ;
#11982 = CARTESIAN_POINT ( 'NONE',  ( -84.07438362643999596, 65.17411849586700612, -145.2984795835770058 ) ) ;
#11983 = CONICAL_SURFACE ( 'NONE', #5304, 10.49999999999999467, 0.7853981633974497223 ) ;
#11984 = DIRECTION ( 'NONE',  ( -1.000000000000000000, 0.000000000000000000, -0.000000000000000000 ) ) ;
#11985 = DIRECTION ( 'NONE',  ( 0.000000000000000000, 0.000000000000000000, 1.000000000000000000 ) ) ;
#11986 = ORIENTED_EDGE ( 'NONE', *, *, #10187, .F. ) ;
#11987 = CARTESIAN_POINT ( 'NONE',  ( 57.41329019055577021, 5.000000000000001776, 97.50956111919106206 ) ) ;
#11988 = VECTOR ( 'NONE', #8564, 1000.000000000000000 ) ;
#11989 = LINE ( 'NONE', #13091, #2776 ) ;
#11990 = ADVANCED_FACE ( 'NONE', ( #15248 ), #4643, .T. ) ;
#11991 = ORIENTED_EDGE ( 'NONE', *, *, #3722, .F. ) ;
#11992 = AXIS2_PLACEMENT_3D ( 'NONE', #7189, #9263, #11670 ) ;
#11993 = DIRECTION ( 'NONE',  ( -0.000000000000000000, -0.000000000000000000, -1.000000000000000000 ) ) ;
#11994 = CARTESIAN_POINT ( 'NONE',  ( -2.415777803760090325, -4.359374999999756639, -2.941435367455751848 ) ) ;
#11995 = ORIENTED_EDGE ( 'NONE', *, *, #4575, .T. ) ;
#11996 = EDGE_CURVE ( 'NONE', #8449, #1774, #12181, .T. ) ;
#11997 = APPLICATION_CONTEXT ( 'automotive_design' ) ;
#11998 = ADVANCED_FACE ( 'NONE', ( #15324 ), #273, .F. ) ;
#11999 = CARTESIAN_POINT ( 'NONE',  ( 3.768993168962329054, -0.5381249999999744293, 1.141810966380977455 ) ) ;
#12000 = AXIS2_PLACEMENT_3D ( 'NONE', #61, #1154, #2395 ) ;
#12001 = AXIS2_PLACEMENT_3D ( 'NONE', #1219, #9587, #10677 ) ;
#12002 = DIRECTION ( 'NONE',  ( 0.000000000000000000, 0.000000000000000000, 1.000000000000000000 ) ) ;
#12003 = DIRECTION ( 'NONE',  ( -0.000000000000000000, 0.9922779949676268085, 0.1240337885538713436 ) ) ;
#12004 = ADVANCED_FACE ( 'NONE', ( #2614, #3701, #8429 ), #12233, .T. ) ;
#12005 = DIRECTION ( 'NONE',  ( -2.551930889570660354E-15, 1.000000000000000000, 0.000000000000000000 ) ) ;
#12006 = CARTESIAN_POINT ( 'NONE',  ( 1.682902201845278611, -5.420849775684215999, 2.811263474311217259 ) ) ;
#12007 = FACE_OUTER_BOUND ( 'NONE', #9291, .T. ) ;
#12008 = DIRECTION ( 'NONE',  ( 0.000000000000000000, 1.000000000000000000, 0.000000000000000000 ) ) ;
#12009 = ORIENTED_EDGE ( 'NONE', *, *, #8763, .T. ) ;
#12010 = LINE ( 'NONE', #10846, #12980 ) ;
#12011 = VECTOR ( 'NONE', #4107, 1000.000000000000000 ) ;
#12012 = CIRCLE ( 'NONE', #10768, 2.399999999999999467 ) ;
#12013 = EDGE_CURVE ( 'NONE', #726, #4630, #2694, .T. ) ;
#12014 = VERTEX_POINT ( 'NONE', #2762 ) ;
#12015 = PLANE ( 'NONE',  #10021 ) ;
#12016 = CARTESIAN_POINT ( 'NONE',  ( -3.535952561574606801, -3.053750000000104770, -0.7042925846621640451 ) ) ;
#12017 = ORIENTED_EDGE ( 'NONE', *, *, #1937, .T. ) ;
#12018 = EDGE_LOOP ( 'NONE', ( #9084, #9764 ) ) ;
#12019 = EDGE_CURVE ( 'NONE', #7621, #12917, #1035, .T. ) ;
#12020 = ORIENTED_EDGE ( 'NONE', *, *, #3273, .T. ) ;
#12021 = B_SPLINE_CURVE_WITH_KNOTS ( 'NONE', 3,
 ( #6298, #3795, #9986, #14716, #5200, #11159 ),
 .UNSPECIFIED., .F., .F.,
 ( 4, 2, 4 ),
 ( 1.820537833122031213, 2.555393473688635453, 3.290249114255239693 ),
 .UNSPECIFIED. ) ;
#12022 = ADVANCED_FACE ( 'NONE', ( #10993 ), #362, .T. ) ;
#12023 = DIRECTION ( 'NONE',  ( 0.000000000000000000, -1.000000000000000000, 0.000000000000000000 ) ) ;
#12024 = CYLINDRICAL_SURFACE ( 'NONE', #901, 8.124999999999992895 ) ;
#12025 = DIRECTION ( 'NONE',  ( 0.000000000000000000, 0.000000000000000000, 1.000000000000000000 ) ) ;
#12026 = CIRCLE ( 'NONE', #6100, 4.000000000000000888 ) ;
#12027 = CARTESIAN_POINT ( 'NONE',  ( 17.12895037488186389, -11.00000029085424913, 0.2687305842673423095 ) ) ;
#12028 = AXIS2_PLACEMENT_3D ( 'NONE', #6627, #5451, #14962 ) ;
#12029 = CARTESIAN_POINT ( 'NONE',  ( -90.85838362644000199, 65.17411849586700612, -147.9984795835769944 ) ) ;
#12030 = CARTESIAN_POINT ( 'NONE',  ( 1.342127543875233808, -3.772500000000060805, -3.243584335895732362 ) ) ;
#12031 = CARTESIAN_POINT ( 'NONE',  ( -80.52077156573417938, 0.000000000000000000, -73.34256232478206528 ) ) ;
#12032 = VERTEX_POINT ( 'NONE', #13404 ) ;
#12033 = DIRECTION ( 'NONE',  ( -1.000000000000000000, 0.000000000000000000, 0.000000000000000000 ) ) ;
#12034 = EDGE_LOOP ( 'NONE', ( #5439, #5207, #6381, #1997, #13215 ) ) ;
#12035 = ORIENTED_EDGE ( 'NONE', *, *, #7465, .T. ) ;
#12036 = ORIENTED_EDGE ( 'NONE', *, *, #2209, .F. ) ;
#12037 = ORIENTED_EDGE ( 'NONE', *, *, #12571, .T. ) ;
#12038 = CONICAL_SURFACE ( 'NONE', #5098, 4.500000000000000888, 1.396263401595466691 ) ;
#12039 = CIRCLE ( 'NONE', #12536, 2.500000000000002220 ) ;
#12040 = CARTESIAN_POINT ( 'NONE',  ( -3.527726845254099075, -3.116249999999919140, 0.7030635791094290710 ) ) ;
#12041 = DIRECTION ( 'NONE',  ( 1.000000000000000000, 9.422394424380278809E-16, 0.000000000000000000 ) ) ;
#12042 = DIRECTION ( 'NONE',  ( -1.000000000000000000, 0.000000000000000000, 0.000000000000000000 ) ) ;
#12043 = FACE_OUTER_BOUND ( 'NONE', #7814, .T. ) ;
#12044 = DIRECTION ( 'NONE',  ( 0.8660254037844485886, 0.000000000000000000, -0.4999999999999827360 ) ) ;
#12045 = CARTESIAN_POINT ( 'NONE',  ( -15.50000000000000000, -0.2038245569916614930, 23.94337567297399971 ) ) ;
#12046 = CARTESIAN_POINT ( 'NONE',  ( -54.81638362644100226, 97.99516924618178848, -147.9984795835769944 ) ) ;
#12047 = PRESENTATION_LAYER_ASSIGNMENT (  '', '', ( #6609 ) ) ;
#12048 = DIRECTION ( 'NONE',  ( 1.060575238724893480E-16, 0.5000000000000189848, -0.8660254037844277164 ) ) ;
#12049 = CARTESIAN_POINT ( 'NONE',  ( -90.85838362644000199, 65.17411849586700612, -147.9984795835769944 ) ) ;
#12050 = PLANE ( 'NONE',  #12715 ) ;
#12051 = AXIS2_PLACEMENT_3D ( 'NONE', #10027, #1730, #5313 ) ;
#12052 = ORIENTED_EDGE ( 'NONE', *, *, #3984, .T. ) ;
#12053 = AXIS2_PLACEMENT_3D ( 'NONE', #14372, #1430, #13537 ) ;
#12054 = CARTESIAN_POINT ( 'NONE',  ( 16.82703061321707949, -11.72093437952781336, 0.2761868948537983814 ) ) ;
#12055 = VERTEX_POINT ( 'NONE', #6502 ) ;
#12056 = EDGE_LOOP ( 'NONE', ( #15173, #131, #12514, #7904 ) ) ;
#12057 = CARTESIAN_POINT ( 'NONE',  ( -4.435020996998820131, -12.00000029085427045, 69.03723529703216855 ) ) ;
#12058 = CARTESIAN_POINT ( 'NONE',  ( 37.35543536254874653, -3.618985300545107364, 6.000000000000001776 ) ) ;
#12059 = AXIS2_PLACEMENT_3D ( 'NONE', #2612, #203, #446 ) ;
#12060 = CARTESIAN_POINT ( 'NONE',  ( -4.230142555718267694, -0.5304635623730820093, 0.8430117587971442950 ) ) ;
#12061 = B_SPLINE_CURVE_WITH_KNOTS ( 'NONE', 3,
 ( #8322, #3430, #12895, #13068, #6092, #13138, #12191, #3967 ),
 .UNSPECIFIED., .F., .F.,
 ( 4, 2, 2, 4 ),
 ( 0.04315383327195209534, 0.04413750674003968227, 0.04512118020812726227, 0.04708852714430240144 ),
 .UNSPECIFIED. ) ;
#12062 = CIRCLE ( 'NONE', #12305, 8.124999999999992895 ) ;
#12063 = FACE_OUTER_BOUND ( 'NONE', #9843, .T. ) ;
#12064 = CIRCLE ( 'NONE', #11279, 4.500000000000000888 ) ;
#12065 = CARTESIAN_POINT ( 'NONE',  ( -35.27438362644000591, 60.67411849586700612, -79.49847958357700861 ) ) ;
#12066 = CARTESIAN_POINT ( 'NONE',  ( 22.58164641901421632, 11.39999970914575833, -0.3335879563140091153 ) ) ;
#12067 = DIRECTION ( 'NONE',  ( 0.000000000000000000, 0.000000000000000000, -1.000000000000000000 ) ) ;
#12068 = EDGE_CURVE ( 'NONE', #1225, #10774, #7740, .T. ) ;
#12069 = CARTESIAN_POINT ( 'NONE',  ( -12.81835358098578759, 11.39999970914576188, -8.183940086454237317 ) ) ;
#12070 = ORIENTED_EDGE ( 'NONE', *, *, #11871, .F. ) ;
#12071 = AXIS2_PLACEMENT_3D ( 'NONE', #5962, #966, #15076 ) ;
#12072 = CARTESIAN_POINT ( 'NONE',  ( -13.41835358098578723, 11.39999970914575833, -0.3335879563140091153 ) ) ;
#12073 = EDGE_CURVE ( 'NONE', #8497, #2784, #7495, .T. ) ;
#12074 = AXIS2_PLACEMENT_3D ( 'NONE', #14112, #11867, #4730 ) ;
#12075 = VERTEX_POINT ( 'NONE', #1752 ) ;
#12076 = CARTESIAN_POINT ( 'NONE',  ( -15.50000000000000000, -0.4000000000000000222, 19.00000000000000355 ) ) ;
#12077 = CARTESIAN_POINT ( 'NONE',  ( -1.128754118026385589, -3.703125000000009770, 3.725901868457750954 ) ) ;
#12078 = ORIENTED_EDGE ( 'NONE', *, *, #214, .F. ) ;
#12079 = CIRCLE ( 'NONE', #14299, 4.500000000000000888 ) ;
#12080 = CARTESIAN_POINT ( 'NONE',  ( 3.372444421885775423, -0.4995676945082423992, 2.006840812041871924 ) ) ;
#12081 = LINE ( 'NONE', #3247, #5599 ) ;
#12082 = AXIS2_PLACEMENT_3D ( 'NONE', #4018, #6445, #7378 ) ;
#12083 = EDGE_CURVE ( 'NONE', #8800, #1856, #2766, .T. ) ;
#12084 = DIRECTION ( 'NONE',  ( -1.000000000000000000, 0.000000000000000000, 0.000000000000000000 ) ) ;
#12085 = DIRECTION ( 'NONE',  ( 0.000000000000000000, 1.000000000000000000, 0.000000000000000000 ) ) ;
#12086 = DIRECTION ( 'NONE',  ( 0.000000000000000000, 0.000000000000000000, 1.000000000000000000 ) ) ;
#12087 = CARTESIAN_POINT ( 'NONE',  ( -52.77438362643999881, 65.17411849586700612, -147.9984795835769944 ) ) ;
#12088 = DIRECTION ( 'NONE',  ( 1.000000000000000000, 0.000000000000000000, 0.000000000000000000 ) ) ;
#12089 = EDGE_CURVE ( 'NONE', #5361, #3573, #11440, .T. ) ;
#12090 = ORIENTED_EDGE ( 'NONE', *, *, #13708, .T. ) ;
#12091 = DIRECTION ( 'NONE',  ( 0.000000000000000000, 1.000000000000000000, 0.000000000000000000 ) ) ;
#12092 = ORIENTED_EDGE ( 'NONE', *, *, #2143, .F. ) ;
#12093 = DIRECTION ( 'NONE',  ( 0.000000000000000000, 0.000000000000000000, 1.000000000000000000 ) ) ;
#12094 = CARTESIAN_POINT ( 'NONE',  ( 2.229831107420913838, -3.725624999999957776, -2.719112200499365528 ) ) ;
#12095 = ORIENTED_EDGE ( 'NONE', *, *, #8006, .F. ) ;
#12096 = VERTEX_POINT ( 'NONE', #8966 ) ;
#12097 = ORIENTED_EDGE ( 'NONE', *, *, #5246, .T. ) ;
#12098 = ADVANCED_FACE ( 'NONE', ( #2928 ), #13481, .T. ) ;
#12099 = DIRECTION ( 'NONE',  ( -0.000000000000000000, 0.000000000000000000, -1.000000000000000000 ) ) ;
#12100 = CARTESIAN_POINT ( 'NONE',  ( -0.3745637740607890565, -5.173691999402833197, -3.583788933605721816 ) ) ;
#12101 = EDGE_CURVE ( 'NONE', #12468, #11318, #2846, .T. ) ;
#12102 = DIRECTION ( 'NONE',  ( 1.000000000000000000, 0.000000000000000000, 0.000000000000000000 ) ) ;
#12103 = DIRECTION ( 'NONE',  ( 0.000000000000000000, 0.000000000000000000, 1.000000000000000000 ) ) ;
#12104 = DIRECTION ( 'NONE',  ( -1.000000000000000000, 0.000000000000000000, -0.000000000000000000 ) ) ;
#12105 = DIRECTION ( 'NONE',  ( 0.000000000000000000, 0.000000000000000000, 1.000000000000000000 ) ) ;
#12106 = EDGE_CURVE ( 'NONE', #12948, #6290, #10194, .T. ) ;
#12107 = DIRECTION ( 'NONE',  ( 1.000000000000000000, 0.000000000000000000, 0.000000000000000000 ) ) ;
#12108 = EDGE_CURVE ( 'NONE', #9101, #4411, #3261, .T. ) ;
#12109 = ORIENTED_EDGE ( 'NONE', *, *, #4472, .T. ) ;
#12110 = DIRECTION ( 'NONE',  ( -1.287488025362404182E-15, -1.000000000000000000, 0.000000000000000000 ) ) ;
#12111 = ORIENTED_EDGE ( 'NONE', *, *, #6979, .F. ) ;
#12112 = ORIENTED_EDGE ( 'NONE', *, *, #5728, .F. ) ;
#12113 = ORIENTED_EDGE ( 'NONE', *, *, #5274, .F. ) ;
#12114 = VERTEX_POINT ( 'NONE', #586 ) ;
#12115 = CIRCLE ( 'NONE', #472, 0.5000000000000000000 ) ;
#12116 = CARTESIAN_POINT ( 'NONE',  ( 15.50000000000000000, -2.500000000000000000, -23.94337567297399971 ) ) ;
#12117 = CARTESIAN_POINT ( 'NONE',  ( -2.896649075160178111, -1.975624999999826548, -2.378478989283399514 ) ) ;
#12118 = CARTESIAN_POINT ( 'NONE',  ( -3.466918327573330849, -3.421874999999993339, -1.851480974780293387 ) ) ;
#12119 = CARTESIAN_POINT ( 'NONE',  ( 0.000000000000000000, 0.000000000000000000, 6.000000000000000000 ) ) ;
#12120 = EDGE_CURVE ( 'NONE', #3694, #3399, #13707, .T. ) ;
#12121 = CARTESIAN_POINT ( 'NONE',  ( 35.35543536254876074, -19.31989681812820692, 0.000000000000000000 ) ) ;
#12122 = DIRECTION ( 'NONE',  ( 0.000000000000000000, 0.000000000000000000, 1.000000000000000000 ) ) ;
#12123 = CARTESIAN_POINT ( 'NONE',  ( -59.02799568714584666, 60.67411849586701322, -79.59847958357700293 ) ) ;
#12124 = CARTESIAN_POINT ( 'NONE',  ( 12.30141533273650900, -8.891480818932939924E-16, 55.44770860939965473 ) ) ;
#12125 = LINE ( 'NONE', #1182, #11538 ) ;
#12126 = DIRECTION ( 'NONE',  ( 0.000000000000000000, 0.000000000000000000, 1.000000000000000000 ) ) ;
#12127 = AXIS2_PLACEMENT_3D ( 'NONE', #8811, #1450, #6204 ) ;
#12128 = EDGE_LOOP ( 'NONE', ( #410, #6081, #534, #155, #798, #6969, #7688, #5868, #4032 ) ) ;
#12129 = LINE ( 'NONE', #1498, #1670 ) ;
#12130 = ORIENTED_EDGE ( 'NONE', *, *, #2320, .T. ) ;
#12131 = ORIENTED_EDGE ( 'NONE', *, *, #3459, .F. ) ;
#12132 = CARTESIAN_POINT ( 'NONE',  ( 3.270563417710623089, -5.585000000000047038, 0.0008246681304770143647 ) ) ;
#12133 = LINE ( 'NONE', #14825, #3506 ) ;
#12134 = CARTESIAN_POINT ( 'NONE',  ( -1.593139518311427194, -1.686713562373179487, 3.843294861269374252 ) ) ;
#12135 = DIRECTION ( 'NONE',  ( 0.000000000000000000, 0.000000000000000000, 1.000000000000000000 ) ) ;
#12136 = FACE_OUTER_BOUND ( 'NONE', #3686, .T. ) ;
#12137 = CARTESIAN_POINT ( 'NONE',  ( -54.81638362644000040, 66.35306774555222376, -147.9984795835769944 ) ) ;
#12138 = LINE ( 'NONE', #6261, #3906 ) ;
#12139 = DIRECTION ( 'NONE',  ( 0.000000000000000000, -1.000000000000000000, 0.000000000000000000 ) ) ;
#12140 = LINE ( 'NONE', #8638, #3243 ) ;
#12141 = EDGE_LOOP ( 'NONE', ( #12850, #13054, #8548, #4335, #9994 ) ) ;
#12142 = CARTESIAN_POINT ( 'NONE',  ( -69.77438362644100778, 92.17411849586700612, -79.49847958357700861 ) ) ;
#12143 = ORIENTED_EDGE ( 'NONE', *, *, #5824, .F. ) ;
#12144 = CARTESIAN_POINT ( 'NONE',  ( 3.568675334318531345, -3.937499999999699796, 1.476665218992084139 ) ) ;
#12145 = VERTEX_POINT ( 'NONE', #9971 ) ;
#12146 = CARTESIAN_POINT ( 'NONE',  ( -3.350768293094503303, -4.421088562373000741, -1.789444311552624400 ) ) ;
#12147 = CARTESIAN_POINT ( 'NONE',  ( -3.204583014436136690, -1.178749999999988640, 2.140022251743640691 ) ) ;
#12148 = ADVANCED_FACE ( 'NONE', ( #14783 ), #14701, .F. ) ;
#12149 = CARTESIAN_POINT ( 'NONE',  ( -75.01311196519617397, 67.29799558322736175, -81.84847958357697451 ) ) ;
#12150 = LINE ( 'NONE', #14695, #9970 ) ;
#12151 = LINE ( 'NONE', #441, #2089 ) ;
#12152 = FACE_OUTER_BOUND ( 'NONE', #5516, .T. ) ;
#12153 = DIRECTION ( 'NONE',  ( -0.000000000000000000, 1.000000000000000000, 0.000000000000000000 ) ) ;
#12154 = LINE ( 'NONE', #7361, #11551 ) ;
#12155 = ORIENTED_EDGE ( 'NONE', *, *, #1529, .F. ) ;
#12156 = ORIENTED_EDGE ( 'NONE', *, *, #2432, .T. ) ;
#12157 = CARTESIAN_POINT ( 'NONE',  ( 15.50000000000000000, -0.2038245569916604938, -21.05662432702600029 ) ) ;
#12158 = CARTESIAN_POINT ( 'NONE',  ( -3.527726845254099519, -3.116249999999919140, 0.7030635791094292930 ) ) ;
#12159 = ORIENTED_EDGE ( 'NONE', *, *, #13188, .F. ) ;
#12160 = PRODUCT_RELATED_PRODUCT_CATEGORY ( 'part', '', ( #9565 ) ) ;
#12161 = ORIENTED_EDGE ( 'NONE', *, *, #595, .T. ) ;
#12162 = EDGE_CURVE ( 'NONE', #1551, #14906, #11689, .T. ) ;
#12163 = DIRECTION ( 'NONE',  ( 0.000000000000000000, 0.000000000000000000, 1.000000000000000000 ) ) ;
#12164 = AXIS2_PLACEMENT_3D ( 'NONE', #11055, #498, #9720 ) ;
#12165 = CARTESIAN_POINT ( 'NONE',  ( -3.372107705793691235, -5.256639709918796477, -0.9200269475832475452 ) ) ;
#12166 = FACE_OUTER_BOUND ( 'NONE', #8839, .T. ) ;
#12167 = VECTOR ( 'NONE', #9248, 1000.000000000000000 ) ;
#12168 = CARTESIAN_POINT ( 'NONE',  ( -1.006616814747114065E-29, -2.568816543514387226E-44, 0.000000000000000000 ) ) ;
#12169 = FACE_BOUND ( 'NONE', #13586, .T. ) ;
#12170 = CARTESIAN_POINT ( 'NONE',  ( -15.50000000000000000, -0.4000000000005236034, 22.50000000000000000 ) ) ;
#12171 = CARTESIAN_POINT ( 'NONE',  ( 15.50000000000000000, -2.500000000000000000, -23.94337567297399971 ) ) ;
#12172 = EDGE_CURVE ( 'NONE', #389, #191, #5014, .T. ) ;
#12173 = EDGE_LOOP ( 'NONE', ( #6282, #1476, #8989, #96 ) ) ;
#12174 = ORIENTED_EDGE ( 'NONE', *, *, #398, .T. ) ;
#12175 = VERTEX_POINT ( 'NONE', #3155 ) ;
#12176 = VERTEX_POINT ( 'NONE', #5185 ) ;
#12177 = VERTEX_POINT ( 'NONE', #14928 ) ;
#12178 = ADVANCED_FACE ( 'NONE', ( #3000 ), #14623, .T. ) ;
#12179 = AXIS2_PLACEMENT_3D ( 'NONE', #11432, #5554, #2120 ) ;
#12180 = LINE ( 'NONE', #12343, #11507 ) ;
#12181 = CIRCLE ( 'NONE', #4262, 4.499999999999997335 ) ;
#12182 = CARTESIAN_POINT ( 'NONE',  ( 3.515159614179530045, -2.538124999999942677, 1.067305873498098912 ) ) ;
#12183 = ADVANCED_FACE ( 'NONE', ( #13565 ), #11298, .T. ) ;
#12184 = EDGE_CURVE ( 'NONE', #181, #14839, #1829, .T. ) ;
#12185 = PRESENTATION_STYLE_ASSIGNMENT (( #2648 ) ) ;
#12186 = CARTESIAN_POINT ( 'NONE',  ( -3.018109139697564114, -3.609375000000057732, 2.478742592228960095 ) ) ;
#12187 = DIRECTION ( 'NONE',  ( 0.1305261922200519342, 0.9914448613738104932, 1.598484835071818104E-17 ) ) ;
#12188 = CARTESIAN_POINT ( 'NONE',  ( 22.58164641901421632, -12.00000029085423670, -11.73358795631401463 ) ) ;
#12189 = CIRCLE ( 'NONE', #1536, 3.968749999999992895 ) ;
#12190 = CARTESIAN_POINT ( 'NONE',  ( -4.781720599710164166, 2.058119353682382524, -0.7178169737032800146 ) ) ;
#12191 = CARTESIAN_POINT ( 'NONE',  ( -73.03793661008894844, 89.17411849586700612, -44.70344037800717274 ) ) ;
#12192 = DIRECTION ( 'NONE',  ( 0.000000000000000000, 0.000000000000000000, 1.000000000000000000 ) ) ;
#12193 = DIRECTION ( 'NONE',  ( 0.000000000000000000, 0.000000000000000000, 1.000000000000000000 ) ) ;
#12194 = AXIS2_PLACEMENT_3D ( 'NONE', #1379, #207, #9659 ) ;
#12195 = EDGE_CURVE ( 'NONE', #9170, #10367, #13927, .T. ) ;
#12196 = ORIENTED_EDGE ( 'NONE', *, *, #12238, .T. ) ;
#12197 = CARTESIAN_POINT ( 'NONE',  ( -62.02799568714584666, 164.3482369917340122, -73.34256232478206528 ) ) ;
#12198 = VECTOR ( 'NONE', #6966, 1000.000000000000000 ) ;
#12199 = ORIENTED_EDGE ( 'NONE', *, *, #11056, .F. ) ;
#12200 = EDGE_LOOP ( 'NONE', ( #5593, #14256, #6787, #5135 ) ) ;
#12201 = ORIENTED_EDGE ( 'NONE', *, *, #3843, .F. ) ;
#12202 = CARTESIAN_POINT ( 'NONE',  ( -52.77438362644000591, 99.17411849586700612, -145.4984795835769660 ) ) ;
#12203 = ADVANCED_FACE ( 'NONE', ( #8263 ), #1124, .F. ) ;
#12204 = CIRCLE ( 'NONE', #8728, 1.449999999999999956 ) ;
#12205 = CARTESIAN_POINT ( 'NONE',  ( 2.894038744318264023, -5.506874999999972431, 1.545501402921600764 ) ) ;
#12206 = AXIS2_PLACEMENT_3D ( 'NONE', #3077, #10504, #4629 ) ;
#12207 = DIRECTION ( 'NONE',  ( 0.000000000000000000, 0.000000000000000000, -1.000000000000000000 ) ) ;
#12208 = CARTESIAN_POINT ( 'NONE',  ( -86.77438362643999881, 62.81621999649657084, -150.4984795835770228 ) ) ;
#12209 = AXIS2_PLACEMENT_3D ( 'NONE', #12920, #5886, #3381 ) ;
#12210 = DIRECTION ( 'NONE',  ( 0.000000000000000000, 1.000000000000000000, 0.000000000000000000 ) ) ;
#12211 = CARTESIAN_POINT ( 'NONE',  ( -69.77438362644001302, 82.17411849586700612, -152.4984795835769944 ) ) ;
#12212 = CARTESIAN_POINT ( 'NONE',  ( -52.77438362644100067, 99.17411849586700612, -145.4984795835769944 ) ) ;
#12213 = CARTESIAN_POINT ( 'NONE',  ( 0.000000000000000000, 0.000000000000000000, -79.59847958357700293 ) ) ;
#12214 = EDGE_LOOP ( 'NONE', ( #14137, #10259 ) ) ;
#12215 = DIRECTION ( 'NONE',  ( 0.000000000000000000, 0.000000000000000000, -1.000000000000000000 ) ) ;
#12216 = CIRCLE ( 'NONE', #312, 0.8000000000000113687 ) ;
#12217 = ORIENTED_EDGE ( 'NONE', *, *, #8743, .F. ) ;
#12218 = AXIS2_PLACEMENT_3D ( 'NONE', #5045, #7305, #12033 ) ;
#12219 = FACE_OUTER_BOUND ( 'NONE', #4432, .T. ) ;
#12220 = CARTESIAN_POINT ( 'NONE',  ( 1.567576417386008947, -2.187499999999996447, -3.781634774997608250 ) ) ;
#12221 = ORIENTED_EDGE ( 'NONE', *, *, #8558, .T. ) ;
#12222 = VECTOR ( 'NONE', #13885, 1000.000000000000000 ) ;
#12223 = FACE_OUTER_BOUND ( 'NONE', #14721, .T. ) ;
#12224 = CARTESIAN_POINT ( 'NONE',  ( -49.02438362644100067, 99.17411849586700612, -150.4984795835770228 ) ) ;
#12225 = FACE_OUTER_BOUND ( 'NONE', #158, .T. ) ;
#12226 = VECTOR ( 'NONE', #10347, 1000.000000000000000 ) ;
#12227 = CARTESIAN_POINT ( 'NONE',  ( 15.50000000000000000, -5.000000000000000000, -22.50000000000000000 ) ) ;
#12228 = AXIS2_PLACEMENT_3D ( 'NONE', #1294, #6138, #6055 ) ;
#12229 = DIRECTION ( 'NONE',  ( -1.000000000000000000, 0.000000000000000000, 0.000000000000000000 ) ) ;
#12230 = DIRECTION ( 'NONE',  ( 0.000000000000000000, 0.000000000000000000, -1.000000000000000000 ) ) ;
#12231 = CARTESIAN_POINT ( 'NONE',  ( -86.77438362644100778, 99.17411849586700612, -147.9984795835769944 ) ) ;
#12232 = FACE_OUTER_BOUND ( 'NONE', #9862, .T. ) ;
#12233 = PLANE ( 'NONE',  #10958 ) ;
#12234 = B_SPLINE_CURVE_WITH_KNOTS ( 'NONE', 3,
 ( #1771, #9915, #6302, #4254, #7536, #5279 ),
 .UNSPECIFIED., .F., .F.,
 ( 4, 2, 4 ),
 ( 0.0002380763768129734448, 0.7291065797294585815, 1.457975083082104328 ),
 .UNSPECIFIED. ) ;
#12235 = CONICAL_SURFACE ( 'NONE', #7546, 2.042000000000002036, 1.047197551196596965 ) ;
#12236 = EDGE_LOOP ( 'NONE', ( #14342, #7250, #13648, #14854, #14558, #650 ) ) ;
#12237 = ORIENTED_EDGE ( 'NONE', *, *, #11337, .T. ) ;
#12238 = EDGE_CURVE ( 'NONE', #6473, #14750, #9848, .T. ) ;
#12239 = ORIENTED_EDGE ( 'NONE', *, *, #13615, .F. ) ;
#12240 = LINE ( 'NONE', #5190, #6083 ) ;
#12241 = CARTESIAN_POINT ( 'NONE',  ( -0.3615547238505232852, -2.319374999999934239, 3.684823279838035592 ) ) ;
#12242 = ORIENTED_EDGE ( 'NONE', *, *, #15318, .T. ) ;
#12243 = VECTOR ( 'NONE', #789, 1000.000000000000000 ) ;
#12244 = AXIS2_PLACEMENT_3D ( 'NONE', #8604, #6221, #1617 ) ;
#12245 = FACE_OUTER_BOUND ( 'NONE', #12450, .T. ) ;
#12246 = CYLINDRICAL_SURFACE ( 'NONE', #11824, 4.000000000000000888 ) ;
#12247 = DIRECTION ( 'NONE',  ( 0.8660254037844383745, -0.5000000000000003331, 0.000000000000000000 ) ) ;
#12248 = DIRECTION ( 'NONE',  ( -0.000000000000000000, 1.000000000000000000, -0.000000000000000000 ) ) ;
#12249 = DIRECTION ( 'NONE',  ( 1.517216463963902273E-16, -1.000000000000000000, -1.734186353771755353E-15 ) ) ;
#12250 = DIRECTION ( 'NONE',  ( 1.000000000000000000, -0.000000000000000000, 1.224646799147353207E-16 ) ) ;
#12251 = AXIS2_PLACEMENT_3D ( 'NONE', #9828, #6441, #8663 ) ;
#12252 = CIRCLE ( 'NONE', #10753, 3.250000000000016431 ) ;
#12253 = ADVANCED_FACE ( 'NONE', ( #8185 ), #4464, .F. ) ;
#12254 = VECTOR ( 'NONE', #6933, 1000.000000000000000 ) ;
#12255 = CARTESIAN_POINT ( 'NONE',  ( -86.77438362644001302, 65.17411849586700612, -86.49847958357699440 ) ) ;
#12256 = EDGE_LOOP ( 'NONE', ( #11622, #14295 ) ) ;
#12257 = CARTESIAN_POINT ( 'NONE',  ( -30.00000000000000000, -5.000000000000000000, -43.00000000000002132 ) ) ;
#12258 = EDGE_CURVE ( 'NONE', #7132, #6631, #13201, .T. ) ;
#12259 = EDGE_LOOP ( 'NONE', ( #2229, #12967, #13006, #3197 ) ) ;
#12260 = ORIENTED_EDGE ( 'NONE', *, *, #14799, .F. ) ;
#12261 = ORIENTED_EDGE ( 'NONE', *, *, #9338, .F. ) ;
#12262 = VERTEX_POINT ( 'NONE', #11757 ) ;
#12263 = VERTEX_POINT ( 'NONE', #13925 ) ;
#12264 = CYLINDRICAL_SURFACE ( 'NONE', #8525, 2.500000000000002220 ) ;
#12265 = CARTESIAN_POINT ( 'NONE',  ( 3.359686712365983929, -1.506874999999983755, 1.796916873358819222 ) ) ;
#12266 = VECTOR ( 'NONE', #4984, 1000.000000000000000 ) ;
#12267 = CARTESIAN_POINT ( 'NONE',  ( 3.407468303614469285, -3.921874999999769074, 1.822475935421856708 ) ) ;
#12268 = CARTESIAN_POINT ( 'NONE',  ( -38.27438362644000591, 111.1741184958670061, -79.49847958357700861 ) ) ;
#12269 = DIRECTION ( 'NONE',  ( 1.000000000000000000, 0.000000000000000000, -6.982962677686266711E-15 ) ) ;
#12270 = CARTESIAN_POINT ( 'NONE',  ( -69.77438362644001302, 81.46011849586699327, -83.44847958357698303 ) ) ;
#12271 = LINE ( 'NONE', #1643, #7293 ) ;
#12272 = LINE ( 'NONE', #8778, #5342 ) ;
#12273 = EDGE_CURVE ( 'NONE', #6920, #12145, #8242, .T. ) ;
#12274 = DIRECTION ( 'NONE',  ( 0.000000000000000000, -1.000000000000000000, 0.000000000000000000 ) ) ;
#12275 = FACE_OUTER_BOUND ( 'NONE', #5925, .T. ) ;
#12276 = ORIENTED_EDGE ( 'NONE', *, *, #6285, .T. ) ;
#12277 = CARTESIAN_POINT ( 'NONE',  ( -13.41835358098578723, 11.75147157172190049, 0.2664120436859908625 ) ) ;
#12278 = COLOUR_RGB ( '', 0.31764706, 0.68627451, 0.89019608) ;
#12279 = EDGE_CURVE ( 'NONE', #3159, #4603, #14913, .T. ) ;
#12280 = ORIENTED_EDGE ( 'NONE', *, *, #14260, .T. ) ;
#12281 = COLOUR_RGB ( '', 0.31764706, 0.68627451, 0.89019608) ;
#12282 = ORIENTED_EDGE ( 'NONE', *, *, #6136, .T. ) ;
#12283 = ORIENTED_EDGE ( 'NONE', *, *, #5293, .F. ) ;
#12284 = VECTOR ( 'NONE', #3543, 1000.000000000000000 ) ;
#12285 = PRODUCT_DEFINITION_CONTEXT ( 'detailed design', #9899, 'design' ) ;
#12286 = CARTESIAN_POINT ( 'NONE',  ( -0.6461339251375918247, -5.303750000000252207, 3.244047683681893890 ) ) ;
#12287 = CARTESIAN_POINT ( 'NONE',  ( 2.729225460314726348, -5.491250000000120757, 1.824606648063345826 ) ) ;
#12288 = ADVANCED_FACE ( 'NONE', ( #2060 ), #5532, .F. ) ;
#12289 = DIRECTION ( 'NONE',  ( -1.000000000000000000, 0.000000000000000000, 0.000000000000000000 ) ) ;
#12290 = AXIS2_PLACEMENT_3D ( 'NONE', #2888, #13744, #1645 ) ;
#12291 = LINE ( 'NONE', #8160, #5261 ) ;
#12292 = CARTESIAN_POINT ( 'NONE',  ( 14.66434062215688883, -0.3156604612129108589, -23.46090750622545684 ) ) ;
#12293 = VECTOR ( 'NONE', #7945, 1000.000000000000000 ) ;
#12294 = DIRECTION ( 'NONE',  ( 1.000000000000000000, 0.000000000000000000, 0.000000000000000000 ) ) ;
#12295 = CARTESIAN_POINT ( 'NONE',  ( 14.25000000000000000, -2.500000000000000000, 23.22168783648699986 ) ) ;
#12296 = AXIS2_PLACEMENT_3D ( 'NONE', #14388, #8507, #3932 ) ;
#12297 = EDGE_CURVE ( 'NONE', #3822, #3973, #6809, .T. ) ;
#12298 = DIRECTION ( 'NONE',  ( 0.000000000000000000, 0.000000000000000000, -1.000000000000000000 ) ) ;
#12299 = ORIENTED_EDGE ( 'NONE', *, *, #3081, .T. ) ;
#12300 = CARTESIAN_POINT ( 'NONE',  ( 15.50000000000000000, -0.4000000000005274892, 22.50000000000000000 ) ) ;
#12301 = ADVANCED_FACE ( 'NONE', ( #10420 ), #8112, .F. ) ;
#12302 = ADVANCED_FACE ( 'NONE', ( #14085 ), #12848, .T. ) ;
#12303 = AXIS2_PLACEMENT_3D ( 'NONE', #3969, #1790, #7557 ) ;
#12304 = ORIENTED_EDGE ( 'NONE', *, *, #2953, .T. ) ;
#12305 = AXIS2_PLACEMENT_3D ( 'NONE', #8002, #12662, #15125 ) ;
#12306 = LINE ( 'NONE', #11062, #7822 ) ;
#12307 = CARTESIAN_POINT ( 'NONE',  ( -0.3862366009529625832, -3.265625000000082601, -3.932116680993492874 ) ) ;
#12308 = EDGE_LOOP ( 'NONE', ( #9115, #4736, #6251, #9131, #3804, #8451, #2497, #1982, #3143, #13372, #8665, #8402, #2771, #4772, #2207, #4299, #1994, #13504, #5359, #10975, #2410, #2331, #15155, #3394 ) ) ;
#12309 = AXIS2_PLACEMENT_3D ( 'NONE', #1097, #2482, #9539 ) ;
#12310 = CARTESIAN_POINT ( 'NONE',  ( -0.7578321119627449143, -3.717963562373217012, 3.817165255294980408 ) ) ;
#12311 = CARTESIAN_POINT ( 'NONE',  ( -1.151041666666718033, 7.362499999999999822, -1.409619492768633328E-16 ) ) ;
#12312 = DIRECTION ( 'NONE',  ( 0.08715574274766176022, 0.000000000000000000, -0.9961946980917453232 ) ) ;
#12313 = DIRECTION ( 'NONE',  ( 0.000000000000000000, -1.000000000000000000, 0.000000000000000000 ) ) ;
#12314 = VECTOR ( 'NONE', #9490, 1000.000000000000000 ) ;
#12315 = DIRECTION ( 'NONE',  ( 0.000000000000000000, 0.000000000000000000, -1.000000000000000000 ) ) ;
#12316 = AXIS2_PLACEMENT_3D ( 'NONE', #697, #8923, #925 ) ;
#12317 = DIRECTION ( 'NONE',  ( -0.000000000000000000, -0.000000000000000000, -1.000000000000000000 ) ) ;
#12318 = DIRECTION ( 'NONE',  ( 1.000000000000000000, 0.000000000000000000, 0.000000000000000000 ) ) ;
#12319 = CARTESIAN_POINT ( 'NONE',  ( 15.50000000000000000, -1.037157890325000054, 26.00000000000000000 ) ) ;
#12320 = CARTESIAN_POINT ( 'NONE',  ( -86.77438362644001302, 59.67411849586700612, -15.85886927678779834 ) ) ;
#12321 = DIRECTION ( 'NONE',  ( -1.000000000000000000, 0.000000000000000000, 0.000000000000000000 ) ) ;
#12322 = EDGE_LOOP ( 'NONE', ( #8230, #3207 ) ) ;
#12323 = VERTEX_POINT ( 'NONE', #2210 ) ;
#12324 = CARTESIAN_POINT ( 'NONE',  ( 17.12895037488186389, -11.00000029085424913, 0.2687305842673423095 ) ) ;
#12325 = CARTESIAN_POINT ( 'NONE',  ( -3.284049251726959717, -2.163124999999908482, 1.754264853118110645 ) ) ;
#12326 = ORIENTED_EDGE ( 'NONE', *, *, #11048, .F. ) ;
#12327 = AXIS2_PLACEMENT_3D ( 'NONE', #13908, #12827, #10333 ) ;
#12328 = CIRCLE ( 'NONE', #5647, 2.700000000000001066 ) ;
#12329 = DIRECTION ( 'NONE',  ( 0.8660254037844482555, 0.000000000000000000, 0.4999999999999831801 ) ) ;
#12330 = CYLINDRICAL_SURFACE ( 'NONE', #6315, 16.00000000000000000 ) ;
#12331 = CARTESIAN_POINT ( 'NONE',  ( 0.6247369625527983139, -0.4995676945082569986, -4.086673213606401234 ) ) ;
#12332 = SURFACE_STYLE_USAGE ( .BOTH. , #5199 ) ;
#12333 = LINE ( 'NONE', #4966, #6112 ) ;
#12334 = DIRECTION ( 'NONE',  ( -1.000000000000000000, -0.000000000000000000, -0.000000000000000000 ) ) ;
#12335 = AXIS2_PLACEMENT_3D ( 'NONE', #1585, #1887, #6642 ) ;
#12336 = ORIENTED_EDGE ( 'NONE', *, *, #7354, .F. ) ;
#12337 = CARTESIAN_POINT ( 'NONE',  ( 15.50000000000000000, -0.2038245569916610489, -23.94337567297399971 ) ) ;
#12338 = ORIENTED_EDGE ( 'NONE', *, *, #14520, .F. ) ;
#12339 = ORIENTED_EDGE ( 'NONE', *, *, #13598, .T. ) ;
#12340 = ORIENTED_EDGE ( 'NONE', *, *, #11526, .F. ) ;
#12341 = ORIENTED_EDGE ( 'NONE', *, *, #10629, .T. ) ;
#12342 = ORIENTED_EDGE ( 'NONE', *, *, #6637, .T. ) ;
#12343 = CARTESIAN_POINT ( 'NONE',  ( 1.634139617129772404, 11.99999970914575798, -0.3335879563140092818 ) ) ;
#12344 = EDGE_CURVE ( 'NONE', #1952, #11360, #6029, .T. ) ;
#12345 = CARTESIAN_POINT ( 'NONE',  ( 2.100337907687909400, -1.741249999999995968, -3.141606438102765075 ) ) ;
#12346 = VECTOR ( 'NONE', #999, 1000.000000000000000 ) ;
#12347 = PRESENTATION_STYLE_ASSIGNMENT (( #7695 ) ) ;
#12348 = CARTESIAN_POINT ( 'NONE',  ( 3.837491448225466062, -3.984374999999830802, 0.3765428855677108166 ) ) ;
#12349 = CARTESIAN_POINT ( 'NONE',  ( 14.25000000000000000, -0.3156864504677152627, -22.74361999681790536 ) ) ;
#12350 = ADVANCED_FACE ( 'NONE', ( #9113 ), #11525, .F. ) ;
#12351 = CARTESIAN_POINT ( 'NONE',  ( 15.91434062215687284, -0.3156604612129197962, 21.29584399676445727 ) ) ;
#12352 = CARTESIAN_POINT ( 'NONE',  ( -38.27438362644000591, 57.67411849586700612, -79.49847958357700861 ) ) ;
#12353 = DIRECTION ( 'NONE',  ( 9.422394424380278809E-16, -1.000000000000000000, 0.000000000000000000 ) ) ;
#12354 = CARTESIAN_POINT ( 'NONE',  ( 15.50000000000000000, -0.2038245569916610489, 21.05662432702600029 ) ) ;
#12355 = DIRECTION ( 'NONE',  ( 0.000000000000000000, 1.000000000000000000, 0.000000000000000000 ) ) ;
#12356 = CARTESIAN_POINT ( 'NONE',  ( -68.09912303623625007, 89.17411849586702033, -44.18949531478481418 ) ) ;
#12357 = SHAPE_REPRESENTATION ( 'MAIN GRIPPER BODY ENCLOSURE', ( #1538, #3518, #12194, #13447 ), #14416 ) ;
#12358 = ORIENTED_EDGE ( 'NONE', *, *, #5293, .T. ) ;
#12359 = CARTESIAN_POINT ( 'NONE',  ( -2.093999815491831562, 9.249999999999998224, 2.564410171457219719E-16 ) ) ;
#12360 = ORIENTED_EDGE ( 'NONE', *, *, #4140, .F. ) ;
#12361 = CIRCLE ( 'NONE', #14088, 3.000000000000000888 ) ;
#12362 = VERTEX_POINT ( 'NONE', #3528 ) ;
#12363 = EDGE_LOOP ( 'NONE', ( #12886, #6667, #14821, #8264 ) ) ;
#12364 = CARTESIAN_POINT ( 'NONE',  ( -3.146746057716334199, -6.053749999999687326, -0.6267477053013468247 ) ) ;
#12365 = CARTESIAN_POINT ( 'NONE',  ( -86.77438362643999881, 65.17411849586700612, -147.9984795835769944 ) ) ;
#12366 = ADVANCED_FACE ( 'NONE', ( #10270 ), #3039, .F. ) ;
#12367 = ADVANCED_FACE ( 'NONE', ( #891 ), #7977, .F. ) ;
#12368 = CARTESIAN_POINT ( 'NONE',  ( 0.3183433322350289751, -5.819374999999986642, -3.223879781222067642 ) ) ;
#12369 = FACE_OUTER_BOUND ( 'NONE', #12906, .T. ) ;
#12370 = CARTESIAN_POINT ( 'NONE',  ( -86.77438362644001302, 59.67411849586700612, -15.85886927678779834 ) ) ;
#12371 = CARTESIAN_POINT ( 'NONE',  ( 68.41329019055577021, 0.000000000000000000, 91.50956111919110469 ) ) ;
#12372 = AXIS2_PLACEMENT_3D ( 'NONE', #11075, #14618, #10910 ) ;
#12373 = DIRECTION ( 'NONE',  ( -0.8660254037844387076, -0.4999999999999998890, 0.000000000000000000 ) ) ;
#12374 = DIRECTION ( 'NONE',  ( 0.000000000000000000, 0.000000000000000000, -1.000000000000000000 ) ) ;
#12375 = CARTESIAN_POINT ( 'NONE',  ( -2.589953986283601850, -4.975625000000236220, -2.126619835350766152 ) ) ;
#12376 = ORIENTED_EDGE ( 'NONE', *, *, #13434, .T. ) ;
#12377 = CARTESIAN_POINT ( 'NONE',  ( 14.66242688423474583, -0.3152598339554803508, 23.45980260912095616 ) ) ;
#12378 = EDGE_CURVE ( 'NONE', #5260, #13566, #15232, .T. ) ;
#12379 = EDGE_CURVE ( 'NONE', #8742, #1201, #4858, .T. ) ;
#12380 = ORIENTED_EDGE ( 'NONE', *, *, #12162, .T. ) ;
#12381 = DIRECTION ( 'NONE',  ( 0.000000000000000000, 4.336808689942017736E-16, -1.000000000000000000 ) ) ;
#12382 = CARTESIAN_POINT ( 'NONE',  ( 0.7730394778201963302, -3.218749999999914735, -3.881000975522858720 ) ) ;
#12383 = EDGE_LOOP ( 'NONE', ( #633, #5363, #9310 ) ) ;
#12384 = EDGE_CURVE ( 'NONE', #7524, #4480, #11989, .T. ) ;
#12385 = LINE ( 'NONE', #1678, #1512 ) ;
#12386 = EDGE_CURVE ( 'NONE', #5514, #13967, #11449, .T. ) ;
#12387 = CARTESIAN_POINT ( 'NONE',  ( -37.27438362644100778, 101.6741184958670061, -79.59847958357700293 ) ) ;
#12388 = EDGE_CURVE ( 'NONE', #1628, #4275, #109, .T. ) ;
#12389 = CARTESIAN_POINT ( 'NONE',  ( -79.11147769456633227, 68.38713492810558137, -83.44847958357698303 ) ) ;
#12390 = PLANE ( 'NONE',  #10887 ) ;
#12391 = CARTESIAN_POINT ( 'NONE',  ( 21.98164641901421135, 11.39999970914575833, -0.3335879563140091153 ) ) ;
#12392 = CARTESIAN_POINT ( 'NONE',  ( 22.58164641901421632, -2.908542394189813650E-07, -11.73358795631400930 ) ) ;
#12393 = CARTESIAN_POINT ( 'NONE',  ( -15.50000000000000000, -0.2000000000000000111, -25.79999999999947136 ) ) ;
#12394 = DIRECTION ( 'NONE',  ( -1.000000000000000000, 0.000000000000000000, 0.000000000000000000 ) ) ;
#12395 = ADVANCED_FACE ( 'NONE', ( #10745 ), #7752, .F. ) ;
#12396 = ORIENTED_EDGE ( 'NONE', *, *, #11431, .T. ) ;
#12397 = ORIENTED_EDGE ( 'NONE', *, *, #9335, .F. ) ;
#12398 = CARTESIAN_POINT ( 'NONE',  ( -15.50000000000000000, -5.000000000000000000, -18.50000000000000000 ) ) ;
#12399 = CARTESIAN_POINT ( 'NONE',  ( -3.579091221414612445, -2.038125000000108322, -1.084269867492464678 ) ) ;
#12400 = ORIENTED_EDGE ( 'NONE', *, *, #11303, .F. ) ;
#12401 = EDGE_CURVE ( 'NONE', #11742, #5737, #1170, .T. ) ;
#12402 = CARTESIAN_POINT ( 'NONE',  ( -48.27438362644000591, 65.17411849586700612, -152.4984795835769944 ) ) ;
#12403 = CARTESIAN_POINT ( 'NONE',  ( -2.355616408154719732, -5.216657250684392011, -2.652406391797293761 ) ) ;
#12404 = CARTESIAN_POINT ( 'NONE',  ( -84.07438362644101915, 99.17411849586700612, -145.4984795835769944 ) ) ;
#12405 = CARTESIAN_POINT ( 'NONE',  ( -85.75338362644100698, 97.40569462133917966, -147.9984795835769944 ) ) ;
#12406 = FILL_AREA_STYLE_COLOUR ( '', #6032 ) ;
#12407 = CARTESIAN_POINT ( 'NONE',  ( 6.573385150445034242, -3.618985300545107364, 6.000000000000001776 ) ) ;
#12408 = CARTESIAN_POINT ( 'NONE',  ( -52.77438362644000591, 65.17411849586700612, -86.49847958357699440 ) ) ;
#12409 = VERTEX_POINT ( 'NONE', #13161 ) ;
#12410 = DIRECTION ( 'NONE',  ( 0.000000000000000000, 0.000000000000000000, 1.000000000000000000 ) ) ;
#12411 = EDGE_LOOP ( 'NONE', ( #540, #1932 ) ) ;
#12412 = VERTEX_POINT ( 'NONE', #7263 ) ;
#12413 = ORIENTED_EDGE ( 'NONE', *, *, #13781, .F. ) ;
#12414 = ORIENTED_EDGE ( 'NONE', *, *, #10001, .T. ) ;
#12415 = ORIENTED_EDGE ( 'NONE', *, *, #3763, .T. ) ;
#12416 = CARTESIAN_POINT ( 'NONE',  ( -75.01311196519617397, 67.29799558322736175, -81.84847958357697451 ) ) ;
#12417 = CARTESIAN_POINT ( 'NONE',  ( 1.740706783794652379, -2.413124999999917808, 3.253752085064650412 ) ) ;
#12418 = DIRECTION ( 'NONE',  ( 0.000000000000000000, 1.000000000000000000, 0.000000000000000000 ) ) ;
#12419 = CARTESIAN_POINT ( 'NONE',  ( -3.711107677420292905, -4.531250000000010658, 0.7371803430742600582 ) ) ;
#12420 = CYLINDRICAL_SURFACE ( 'NONE', #3537, 2.750000000000002665 ) ;
#12421 = CARTESIAN_POINT ( 'NONE',  ( 10.10406781373725771, -12.00000029085427222, 69.08979243323352648 ) ) ;
#12422 = DIRECTION ( 'NONE',  ( 2.551930889570659960E-15, -1.000000000000000000, -0.000000000000000000 ) ) ;
#12423 = CARTESIAN_POINT ( 'NONE',  ( 2.013502677559834808, -0.8281249999998109290, 3.769415173278118480 ) ) ;
#12424 = CARTESIAN_POINT ( 'NONE',  ( -86.77438362644001302, 65.17411849586700612, -145.4984795835769660 ) ) ;
#12425 = CYLINDRICAL_SURFACE ( 'NONE', #1896, 1.785937500000001066 ) ;
#12426 = DIRECTION ( 'NONE',  ( 0.000000000000000000, -4.336808689942017736E-16, 1.000000000000000000 ) ) ;
#12427 = ORIENTED_EDGE ( 'NONE', *, *, #3757, .F. ) ;
#12428 = DIRECTION ( 'NONE',  ( 1.000000000000000000, 0.000000000000000000, -1.224646799147352468E-16 ) ) ;
#12429 = VERTEX_POINT ( 'NONE', #9316 ) ;
#12430 = AXIS2_PLACEMENT_3D ( 'NONE', #6940, #11658, #3210 ) ;
#12431 = VERTEX_POINT ( 'NONE', #2108 ) ;
#12432 = EDGE_LOOP ( 'NONE', ( #13488, #12130 ) ) ;
#12433 = PRODUCT_DEFINITION_CONTEXT ( 'detailed design', #2768, 'design' ) ;
#12434 = EDGE_CURVE ( 'NONE', #191, #2764, #10633, .T. ) ;
#12435 = DIRECTION ( 'NONE',  ( 0.000000000000000000, 0.000000000000000000, -1.000000000000000000 ) ) ;
#12436 = CARTESIAN_POINT ( 'NONE',  ( -3.146746057716333755, -6.053749999999687326, -0.6267477053013468247 ) ) ;
#12437 = AXIS2_PLACEMENT_3D ( 'NONE', #11068, #5176, #3145 ) ;
#12438 = CARTESIAN_POINT ( 'NONE',  ( -69.77438362644100778, 82.17411849586700612, -67.49847958357700861 ) ) ;
#12439 = DIRECTION ( 'NONE',  ( -1.000000000000000000, -1.747085166004344019E-15, 0.000000000000000000 ) ) ;
#12440 = FACE_OUTER_BOUND ( 'NONE', #1317, .T. ) ;
#12441 = CARTESIAN_POINT ( 'NONE',  ( -37.27438362644000591, 65.17411849586700612, -152.4984795835769944 ) ) ;
#12442 = DIRECTION ( 'NONE',  ( -1.287488025362404182E-15, -1.000000000000000000, 0.000000000000000000 ) ) ;
#12443 = VECTOR ( 'NONE', #6281, 1000.000000000000000 ) ;
#12444 = CARTESIAN_POINT ( 'NONE',  ( -2.933994605034232706, -5.163125000000027498, 1.567297863280144865 ) ) ;
#12445 = ORIENTED_EDGE ( 'NONE', *, *, #13327, .T. ) ;
#12446 = DIRECTION ( 'NONE',  ( 0.000000000000000000, 0.000000000000000000, 1.000000000000000000 ) ) ;
#12447 = EDGE_CURVE ( 'NONE', #14595, #502, #2661, .T. ) ;
#12448 = AXIS2_PLACEMENT_3D ( 'NONE', #767, #4497, #15109 ) ;
#12449 = CONTEXT_DEPENDENT_SHAPE_REPRESENTATION ( #10102, #10680 ) ;
#12450 = EDGE_LOOP ( 'NONE', ( #12413, #9588, #10064 ) ) ;
#12451 = EDGE_CURVE ( 'NONE', #12703, #14576, #13450, .T. ) ;
#12452 = AXIS2_PLACEMENT_3D ( 'NONE', #5336, #1831, #14556 ) ;
#12453 = CARTESIAN_POINT ( 'NONE',  ( 3.641945650916532884, -1.921875000000019540, 1.944964469737308299 ) ) ;
#12454 = ORIENTED_EDGE ( 'NONE', *, *, #14608, .T. ) ;
#12455 = AXIS2_PLACEMENT_3D ( 'NONE', #8691, #1325, #2650 ) ;
#12456 = CARTESIAN_POINT ( 'NONE',  ( -3.447875558419448705, -3.577338562373083342, 1.844546225587363031 ) ) ;
#12457 = LINE ( 'NONE', #11289, #14143 ) ;
#12458 = CARTESIAN_POINT ( 'NONE',  ( -90.85838362644000199, 65.17411849586700612, -147.9984795835769944 ) ) ;
#12459 =( GEOMETRIC_REPRESENTATION_CONTEXT ( 3 ) GLOBAL_UNCERTAINTY_ASSIGNED_CONTEXT ( ( #324 ) ) GLOBAL_UNIT_ASSIGNED_CONTEXT ( ( #9126, #9427, #10435 ) ) REPRESENTATION_CONTEXT ( 'NONE', 'WORKASPACE' ) );
#12460 = CARTESIAN_POINT ( 'NONE',  ( 2.598076211353314235, 0.1227504548087474667, -4.499999999999999112 ) ) ;
#12461 = DIRECTION ( 'NONE',  ( 0.000000000000000000, 0.000000000000000000, -1.000000000000000000 ) ) ;
#12462 = CARTESIAN_POINT ( 'NONE',  ( 0.9018160986460356243, 2.304554878308276766, 4.500000000000000000 ) ) ;
#12463 = CARTESIAN_POINT ( 'NONE',  ( 16.75000000000000000, -2.500000000000000000, 21.77831216351300014 ) ) ;
#12464 = CARTESIAN_POINT ( 'NONE',  ( -59.02799568714584666, 59.67411849586700612, -79.59847958357700293 ) ) ;
#12465 = VECTOR ( 'NONE', #9887, 1000.000000000000114 ) ;
#12466 = EDGE_CURVE ( 'NONE', #3938, #3097, #12657, .T. ) ;
#12467 = DIRECTION ( 'NONE',  ( 1.000000000000000000, 0.000000000000000000, 0.000000000000000000 ) ) ;
#12468 = VERTEX_POINT ( 'NONE', #5852 ) ;
#12469 = ORIENTED_EDGE ( 'NONE', *, *, #4097, .T. ) ;
#12470 = EDGE_CURVE ( 'NONE', #5594, #11761, #11578, .T. ) ;
#12471 = CARTESIAN_POINT ( 'NONE',  ( -101.2743836264399988, 114.1741184958670061, -67.49847958357700861 ) ) ;
#12472 = EDGE_CURVE ( 'NONE', #6145, #12075, #15124, .T. ) ;
#12473 = CARTESIAN_POINT ( 'NONE',  ( -2.463482987169076210, -0.9443750000000532552, -3.003366100166338093 ) ) ;
#12474 = ORIENTED_EDGE ( 'NONE', *, *, #7925, .F. ) ;
#12475 = CIRCLE ( 'NONE', #14445, 9.999999999999994671 ) ;
#12476 = DIRECTION ( 'NONE',  ( -1.000000000000000000, 0.000000000000000000, 0.000000000000000000 ) ) ;
#12477 = AXIS2_PLACEMENT_3D ( 'NONE', #318, #5068, #9780 ) ;
#12478 = ADVANCED_FACE ( 'NONE', ( #4746 ), #15283, .F. ) ;
#12479 = DIRECTION ( 'NONE',  ( 0.000000000000000000, 1.000000000000000000, 0.000000000000000000 ) ) ;
#12480 = CARTESIAN_POINT ( 'NONE',  ( -69.77438362644001302, 82.17411849586700612, -80.14847958357698587 ) ) ;
#12481 = AXIS2_PLACEMENT_3D ( 'NONE', #3738, #7321, #10153 ) ;
#12482 = DIRECTION ( 'NONE',  ( 1.000000000000000000, 2.551930889570660354E-15, 0.000000000000000000 ) ) ;
#12483 = DIRECTION ( 'NONE',  ( 0.000000000000000000, 0.000000000000000000, 1.000000000000000000 ) ) ;
#12484 = DIRECTION ( 'NONE',  ( 0.000000000000000000, 0.000000000000000000, -1.000000000000000000 ) ) ;
#12485 = EDGE_CURVE ( 'NONE', #10868, #14784, #8082, .T. ) ;
#12486 = CYLINDRICAL_SURFACE ( 'NONE', #602, 4.499999999999997335 ) ;
#12487 = ORIENTED_EDGE ( 'NONE', *, *, #421, .T. ) ;
#12488 = DIRECTION ( 'NONE',  ( -0.000000000000000000, 1.000000000000000000, 0.000000000000000000 ) ) ;
#12489 = CIRCLE ( 'NONE', #4804, 8.000000000000007105 ) ;
#12490 = VECTOR ( 'NONE', #9658, 1000.000000000000000 ) ;
#12491 = VERTEX_POINT ( 'NONE', #1176 ) ;
#12492 = ADVANCED_FACE ( 'NONE', ( #4593 ), #5933, .T. ) ;
#12493 = VERTEX_POINT ( 'NONE', #8001 ) ;
#12494 = EDGE_CURVE ( 'NONE', #3825, #10769, #10327, .T. ) ;
#12495 = ORIENTED_EDGE ( 'NONE', *, *, #4389, .F. ) ;
#12496 = ORIENTED_EDGE ( 'NONE', *, *, #5174, .T. ) ;
#12497 = ORIENTED_EDGE ( 'NONE', *, *, #15318, .F. ) ;
#12498 = CARTESIAN_POINT ( 'NONE',  ( -3.508963762376760442, -6.483587779271561935, -0.3443070125793121217 ) ) ;
#12499 = CARTESIAN_POINT ( 'NONE',  ( -0.7729260235471533402, -0.3037499999998679590, 3.893172034236888290 ) ) ;
#12500 = APPLICATION_CONTEXT ( 'automotive_design' ) ;
#12501 = FACE_OUTER_BOUND ( 'NONE', #1258, .T. ) ;
#12502 = CARTESIAN_POINT ( 'NONE',  ( 3.641945650916532884, -1.921875000000019540, 1.944964469737308299 ) ) ;
#12503 = AXIS2_PLACEMENT_3D ( 'NONE', #8433, #6212, #7368 ) ;
#12504 = VECTOR ( 'NONE', #5209, 1000.000000000000000 ) ;
#12505 = CARTESIAN_POINT ( 'NONE',  ( -16.75000000000000000, -0.2714405302574894319, 22.98746066354538087 ) ) ;
#12506 = CARTESIAN_POINT ( 'NONE',  ( -16.75000000000000000, -2.500000000000000000, -23.22168783648699986 ) ) ;
#12507 = CARTESIAN_POINT ( 'NONE',  ( -3.663887442738355205, 2.356280171323974937, -2.653960795963570707 ) ) ;
#12508 = CARTESIAN_POINT ( 'NONE',  ( 0.8221312990109845842, -1.218750000000059952, -4.140949732771461278 ) ) ;
#12509 = CARTESIAN_POINT ( 'NONE',  ( -50.73238362643999722, 66.35306774555222376, -147.9984795835769944 ) ) ;
#12510 = DIRECTION ( 'NONE',  ( -1.000000000000000000, 0.000000000000000000, 0.000000000000000000 ) ) ;
#12511 = PLANE ( 'NONE',  #10235 ) ;
#12512 = ORIENTED_EDGE ( 'NONE', *, *, #1937, .F. ) ;
#12513 = CARTESIAN_POINT ( 'NONE',  ( -4.763139720814411504, 0.04639863247562013571, 0.7499999999999986677 ) ) ;
#12514 = ORIENTED_EDGE ( 'NONE', *, *, #2483, .T. ) ;
#12515 = ORIENTED_EDGE ( 'NONE', *, *, #7169, .T. ) ;
#12516 = ORIENTED_EDGE ( 'NONE', *, *, #4599, .T. ) ;
#12517 = VECTOR ( 'NONE', #12315, 1000.000000000000000 ) ;
#12518 = CARTESIAN_POINT ( 'NONE',  ( -54.81638362644100226, 97.99516924618178848, -147.9984795835769944 ) ) ;
#12519 = CARTESIAN_POINT ( 'NONE',  ( 2.516189350642509037, -5.694375000000295728, -2.066564183454873138 ) ) ;
#12520 = DIRECTION ( 'NONE',  ( -0.000000000000000000, 0.000000000000000000, 1.000000000000000000 ) ) ;
#12521 = CARTESIAN_POINT ( 'NONE',  ( -42.77438362644000591, 65.17411849586700612, -152.4984795835769944 ) ) ;
#12522 = LINE ( 'NONE', #14831, #6859 ) ;
#12523 = DIRECTION ( 'NONE',  ( 1.000000000000000000, 0.000000000000000000, 0.000000000000000000 ) ) ;
#12524 = CARTESIAN_POINT ( 'NONE',  ( -1.623800369386649400, -0.4995676945082628828, 3.803957840413579206 ) ) ;
#12525 = AXIS2_PLACEMENT_3D ( 'NONE', #12149, #13626, #7507 ) ;
#12526 = CARTESIAN_POINT ( 'NONE',  ( 1.879752899984456160, -4.741249999999911147, -2.811701655874830230 ) ) ;
#12527 = ORIENTED_EDGE ( 'NONE', *, *, #12938, .F. ) ;
#12528 = VECTOR ( 'NONE', #3034, 1000.000000000000114 ) ;
#12529 = FACE_OUTER_BOUND ( 'NONE', #2158, .T. ) ;
#12530 = ORIENTED_EDGE ( 'NONE', *, *, #12938, .T. ) ;
#12531 = EDGE_LOOP ( 'NONE', ( #10296, #5965 ) ) ;
#12532 = CARTESIAN_POINT ( 'NONE',  ( 3.968938162104017842, -2.984375000000153211, 0.3919611025626033030 ) ) ;
#12533 = ORIENTED_EDGE ( 'NONE', *, *, #11407, .F. ) ;
#12534 = CARTESIAN_POINT ( 'NONE',  ( 2.152085272744272526, -3.842963562373026942, 3.222648864007900293 ) ) ;
#12535 = AXIS2_PLACEMENT_3D ( 'NONE', #7276, #12002, #11070 ) ;
#12536 = AXIS2_PLACEMENT_3D ( 'NONE', #3878, #13496, #1543 ) ;
#12537 = LINE ( 'NONE', #13624, #8951 ) ;
#12538 = ADVANCED_FACE ( 'NONE', ( #3427 ), #9715, .T. ) ;
#12539 = CARTESIAN_POINT ( 'NONE',  ( -69.77438362644001302, 82.17411849586700612, -138.4984795835769944 ) ) ;
#12540 = CARTESIAN_POINT ( 'NONE',  ( 14.24999999999999822, -0.2715193793361405095, 22.01281590054915327 ) ) ;
#12541 = EDGE_CURVE ( 'NONE', #411, #14750, #4678, .T. ) ;
#12542 = DIRECTION ( 'NONE',  ( 0.000000000000000000, 0.000000000000000000, 1.000000000000000000 ) ) ;
#12543 = CARTESIAN_POINT ( 'NONE',  ( -30.00000000000000000, -5.000000000000000000, -43.00000000000002132 ) ) ;
#12544 = CARTESIAN_POINT ( 'NONE',  ( -3.464101615137753942, -9.164895919936631821E-15, 2.999999999999998668 ) ) ;
#12545 = AXIS2_PLACEMENT_3D ( 'NONE', #552, #5380, #5299 ) ;
#12546 = CARTESIAN_POINT ( 'NONE',  ( 15.50000000000000000, -5.000000000000000000, -26.50000000000000000 ) ) ;
#12547 = CARTESIAN_POINT ( 'NONE',  ( 1.403561989263863629E-14, -5.500000000000003553, 0.000000000000000000 ) ) ;
#12548 = CIRCLE ( 'NONE', #3119, 4.500000000000003553 ) ;
#12549 = AXIS2_PLACEMENT_3D ( 'NONE', #6410, #1728, #1504 ) ;
#12550 = VERTEX_POINT ( 'NONE', #14127 ) ;
#12551 = CARTESIAN_POINT ( 'NONE',  ( 33.35543536254877495, -19.31989681812820692, 6.000000000000001776 ) ) ;
#12552 = CARTESIAN_POINT ( 'NONE',  ( 3.722330097189531006, -1.616249999999942899, -0.7418360188101490449 ) ) ;
#12553 = ORIENTED_EDGE ( 'NONE', *, *, #149, .T. ) ;
#12554 = VECTOR ( 'NONE', #5491, 1000.000000000000000 ) ;
#12555 = DIRECTION ( 'NONE',  ( -1.000000000000000000, 0.000000000000000000, 0.000000000000000000 ) ) ;
#12556 = EDGE_CURVE ( 'NONE', #4383, #2303, #1794, .T. ) ;
#12557 = AXIS2_PLACEMENT_3D ( 'NONE', #4444, #3050, #13833 ) ;
#12558 = FACE_OUTER_BOUND ( 'NONE', #6144, .T. ) ;
#12559 = FACE_OUTER_BOUND ( 'NONE', #13548, .T. ) ;
#12560 = ADVANCED_FACE ( 'NONE', ( #9541 ), #7550, .F. ) ;
#12561 = PLANE ( 'NONE',  #8635 ) ;
#12562 = DIRECTION ( 'NONE',  ( 1.000000000000000000, 0.000000000000000000, 0.000000000000000000 ) ) ;
#12563 = CYLINDRICAL_SURFACE ( 'NONE', #8968, 4.499999999999997335 ) ;
#12564 = ORIENTED_EDGE ( 'NONE', *, *, #3001, .T. ) ;
#12565 = CARTESIAN_POINT ( 'NONE',  ( -80.52077156573417938, 103.6741184958669777, -73.34256232478206528 ) ) ;
#12566 = AXIS2_PLACEMENT_3D ( 'NONE', #9569, #11058, #428 ) ;
#12567 = ORIENTED_EDGE ( 'NONE', *, *, #12766, .F. ) ;
#12568 = EDGE_CURVE ( 'NONE', #11388, #10261, #1246, .T. ) ;
#12569 = ORIENTED_EDGE ( 'NONE', *, *, #2314, .T. ) ;
#12570 = EDGE_LOOP ( 'NONE', ( #8387, #2462, #11657, #9157 ) ) ;
#12571 = EDGE_CURVE ( 'NONE', #7989, #4297, #9958, .T. ) ;
#12572 = ORIENTED_EDGE ( 'NONE', *, *, #6253, .F. ) ;
#12573 = ORIENTED_EDGE ( 'NONE', *, *, #6869, .F. ) ;
#12574 = CARTESIAN_POINT ( 'NONE',  ( 1.033028120569788211, -6.202338562373084230, -3.409978924178418858 ) ) ;
#12575 = CARTESIAN_POINT ( 'NONE',  ( -3.705025434593251177, -1.038125000000020393, -1.124966067554165727 ) ) ;
#12576 = ADVANCED_FACE ( 'NONE', ( #2799 ), #8541, .F. ) ;
#12577 = CARTESIAN_POINT ( 'NONE',  ( -73.13733409597239188, 66.60412428008086749, -83.44847958357698303 ) ) ;
#12578 = CARTESIAN_POINT ( 'NONE',  ( 1.536269025742735383, -2.812500000000037303, 3.705069426614713723 ) ) ;
#12579 = CARTESIAN_POINT ( 'NONE',  ( 14.25000000000000000, -0.2038245569916330158, -23.22168783648699986 ) ) ;
#12580 = LINE ( 'NONE', #4199, #9571 ) ;
#12581 = ADVANCED_FACE ( 'NONE', ( #3813 ), #3277, .T. ) ;
#12582 = AXIS2_PLACEMENT_3D ( 'NONE', #14680, #8872, #11051 ) ;
#12583 = ADVANCED_FACE ( 'NONE', ( #6007, #3892, #5057, #13206, #4913 ), #6314, .F. ) ;
#12584 = DIRECTION ( 'NONE',  ( 0.000000000000000000, 0.000000000000000000, -1.000000000000000000 ) ) ;
#12585 = CARTESIAN_POINT ( 'NONE',  ( 3.803621785104590794E-17, 9.355654565435173708, 0.000000000000000000 ) ) ;
#12586 = FACE_BOUND ( 'NONE', #8388, .T. ) ;
#12587 = CARTESIAN_POINT ( 'NONE',  ( -9.797174393178998714E-17, 9.500000000000000000, 0.000000000000000000 ) ) ;
#12588 = ORIENTED_EDGE ( 'NONE', *, *, #1847, .F. ) ;
#12589 = CARTESIAN_POINT ( 'NONE',  ( -3.897114317029974462, -9.945166405816860437E-15, 2.249999999999999112 ) ) ;
#12590 = ORIENTED_EDGE ( 'NONE', *, *, #10464, .F. ) ;
#12591 = VERTEX_POINT ( 'NONE', #11025 ) ;
#12592 = ORIENTED_EDGE ( 'NONE', *, *, #7647, .F. ) ;
#12593 = VECTOR ( 'NONE', #643, 1000.000000000000000 ) ;
#12594 = CARTESIAN_POINT ( 'NONE',  ( -73.13733409597239188, 66.60412428008086749, -83.44847958357698303 ) ) ;
#12595 = ADVANCED_FACE ( 'NONE', ( #4979 ), #14506, .T. ) ;
#12596 = DIRECTION ( 'NONE',  ( 0.000000000000000000, 0.000000000000000000, 1.000000000000000000 ) ) ;
#12597 = CARTESIAN_POINT ( 'NONE',  ( -69.77438362644001302, 92.37411849586700896, -80.14847958357698587 ) ) ;
#12598 = LINE ( 'NONE', #14976, #10818 ) ;
#12599 = CARTESIAN_POINT ( 'NONE',  ( -67.09329877327485292, 74.51466092244987749, -58.65793715699411592 ) ) ;
#12600 = DIRECTION ( 'NONE',  ( 0.000000000000000000, 1.000000000000000000, 0.000000000000000000 ) ) ;
#12601 = CIRCLE ( 'NONE', #5928, 3.299999999999473577 ) ;
#12602 = CARTESIAN_POINT ( 'NONE',  ( 0.0008557816480155369665, -4.835000000000089670, -3.369777484087370212 ) ) ;
#12603 = ORIENTED_EDGE ( 'NONE', *, *, #5371, .T. ) ;
#12604 = CARTESIAN_POINT ( 'NONE',  ( -37.27438362642642034, 65.17411849586919459, -79.59847958357700293 ) ) ;
#12605 = ORIENTED_EDGE ( 'NONE', *, *, #14984, .F. ) ;
#12606 = DIRECTION ( 'NONE',  ( 0.000000000000000000, 0.000000000000000000, -1.000000000000000000 ) ) ;
#12607 = EDGE_LOOP ( 'NONE', ( #5967, #13585, #6077, #10660, #12995 ) ) ;
#12608 = CARTESIAN_POINT ( 'NONE',  ( 0.8221312990109845842, -1.218750000000059952, -4.140949732771461278 ) ) ;
#12609 = EDGE_LOOP ( 'NONE', ( #2944, #225, #5781, #6633 ) ) ;
#12610 = CARTESIAN_POINT ( 'NONE',  ( -1.561832126663101450, -2.311713562373265862, -3.766729512901092480 ) ) ;
#12611 = VECTOR ( 'NONE', #5899, 1000.000000000000000 ) ;
#12612 = PLANE ( 'NONE',  #5247 ) ;
#12613 = FACE_OUTER_BOUND ( 'NONE', #14687, .T. ) ;
#12614 = DIRECTION ( 'NONE',  ( 0.000000000000000000, 0.000000000000000000, -1.000000000000000000 ) ) ;
#12615 = CARTESIAN_POINT ( 'NONE',  ( -35.58670980944424400, 2.488961461112888074, 95.72362361919107343 ) ) ;
#12616 = FACE_OUTER_BOUND ( 'NONE', #7690, .T. ) ;
#12617 = CARTESIAN_POINT ( 'NONE',  ( -15.50000000000000000, -5.000000000000000000, -22.50000000000000000 ) ) ;
#12618 = DIRECTION ( 'NONE',  ( -0.000000000000000000, 1.000000000000000000, -0.000000000000000000 ) ) ;
#12619 = ORIENTED_EDGE ( 'NONE', *, *, #13799, .F. ) ;
#12620 =( NAMED_UNIT ( * ) PLANE_ANGLE_UNIT ( ) SI_UNIT ( $, .RADIAN. ) );
#12621 = CARTESIAN_POINT ( 'NONE',  ( -3.978984329191358693, -0.08500000000000000611, -3.334211887901014441E-13 ) ) ;
#12622 = ORIENTED_EDGE ( 'NONE', *, *, #1230, .T. ) ;
#12623 = ADVANCED_FACE ( 'NONE', ( #7234 ), #6089, .F. ) ;
#12624 = DIRECTION ( 'NONE',  ( 0.000000000000000000, -1.000000000000000000, 0.000000000000000000 ) ) ;
#12625 = CARTESIAN_POINT ( 'NONE',  ( 17.23697745638123280, -3.616872831399570831, -0.03314156585704653574 ) ) ;
#12626 = CARTESIAN_POINT ( 'NONE',  ( -4.522482571421200248, 10.99999970914572422, 70.03692566716178192 ) ) ;
#12627 = DIRECTION ( 'NONE',  ( 0.000000000000000000, 1.000000000000000000, 0.000000000000000000 ) ) ;
#12628 = DIRECTION ( 'NONE',  ( 0.000000000000000000, 1.000000000000000000, 0.000000000000000000 ) ) ;
#12629 = EDGE_LOOP ( 'NONE', ( #3555, #5591 ) ) ;
#12630 = FACE_OUTER_BOUND ( 'NONE', #12609, .T. ) ;
#12631 = EDGE_CURVE ( 'NONE', #14726, #1497, #9621, .T. ) ;
#12632 = ORIENTED_EDGE ( 'NONE', *, *, #13061, .F. ) ;
#12633 = ORIENTED_EDGE ( 'NONE', *, *, #6506, .T. ) ;
#12634 = CARTESIAN_POINT ( 'NONE',  ( 2.516189350642509481, -5.694375000000295728, -2.066564183454791870 ) ) ;
#12635 = ORIENTED_EDGE ( 'NONE', *, *, #14754, .T. ) ;
#12636 = ORIENTED_EDGE ( 'NONE', *, *, #5474, .T. ) ;
#12637 = ORIENTED_EDGE ( 'NONE', *, *, #6851, .F. ) ;
#12638 = CARTESIAN_POINT ( 'NONE',  ( 3.429681579265138947, -6.046088562373067354, -1.039418128961893117 ) ) ;
#12639 = CARTESIAN_POINT ( 'NONE',  ( -0.7612222386588485268, -0.8662499999999671019, -3.819631723157196568 ) ) ;
#12640 = FACE_BOUND ( 'NONE', #10566, .T. ) ;
#12641 = CARTESIAN_POINT ( 'NONE',  ( -4.030856054181176873, -2.515624999999848121, 0.3959303163381804880 ) ) ;
#12642 = DIRECTION ( 'NONE',  ( 1.000000000000000000, 0.000000000000000000, 0.000000000000000000 ) ) ;
#12643 = DIRECTION ( 'NONE',  ( 0.000000000000000000, 0.000000000000000000, 1.000000000000000000 ) ) ;
#12644 = EDGE_CURVE ( 'NONE', #4454, #3610, #8618, .T. ) ;
#12645 = CARTESIAN_POINT ( 'NONE',  ( 35.35543536254876074, -3.618985300545107364, 0.000000000000000000 ) ) ;
#12646 = CARTESIAN_POINT ( 'NONE',  ( 1.991706217211437036, -1.171874999999983347, -3.729459312589495923 ) ) ;
#12647 = LINE ( 'NONE', #12509, #379 ) ;
#12648 = PLANE ( 'NONE',  #13050 ) ;
#12649 = CARTESIAN_POINT ( 'NONE',  ( 4.362044368365340929, 1.127570259384924611E-14, 5.341963673457352387E-16 ) ) ;
#12650 = ORIENTED_EDGE ( 'NONE', *, *, #4124, .T. ) ;
#12651 = CYLINDRICAL_SURFACE ( 'NONE', #1566, 17.00000000000000000 ) ;
#12652 = ADVANCED_FACE ( 'NONE', ( #12043 ), #14354, .T. ) ;
#12653 = ORIENTED_EDGE ( 'NONE', *, *, #862, .F. ) ;
#12654 = ORIENTED_EDGE ( 'NONE', *, *, #6158, .F. ) ;
#12655 = ORIENTED_EDGE ( 'NONE', *, *, #9297, .T. ) ;
#12656 = ADVANCED_FACE ( 'NONE', ( #3731, #8461, #2722, #1414, #6172 ), #1558, .T. ) ;
#12657 = B_SPLINE_CURVE_WITH_KNOTS ( 'NONE', 3,
 ( #1099, #3499, #7090, #7164, #10477, #5624 ),
 .UNSPECIFIED., .F., .F.,
 ( 4, 2, 4 ),
 ( 1.820537833122031213, 2.555393473688635453, 3.290249114255239693 ),
 .UNSPECIFIED. ) ;
#12658 = CARTESIAN_POINT ( 'NONE',  ( 15.70313394608857394, -0.2715358723588625622, 23.82609623451821079 ) ) ;
#12659 = EDGE_CURVE ( 'NONE', #10438, #11322, #6239, .T. ) ;
#12660 = FACE_OUTER_BOUND ( 'NONE', #8032, .T. ) ;
#12661 = DIRECTION ( 'NONE',  ( 0.000000000000000000, 0.000000000000000000, -1.000000000000000000 ) ) ;
#12662 = DIRECTION ( 'NONE',  ( 0.000000000000000000, 0.000000000000000000, -1.000000000000000000 ) ) ;
#12663 = ADVANCED_FACE ( 'NONE', ( #397 ), #5292, .F. ) ;
#12664 = CARTESIAN_POINT ( 'NONE',  ( -52.77438362643999881, 65.17411849586700612, -147.9984795835769944 ) ) ;
#12665 = CARTESIAN_POINT ( 'NONE',  ( -51.75338362644099277, 97.40569462133917966, -147.9984795835769944 ) ) ;
#12666 = CARTESIAN_POINT ( 'NONE',  ( -52.77438362643999881, 67.53201699523744139, -147.9984795835769944 ) ) ;
#12667 = VECTOR ( 'NONE', #5195, 1000.000000000000000 ) ;
#12668 = VERTEX_POINT ( 'NONE', #3029 ) ;
#12669 = FACE_OUTER_BOUND ( 'NONE', #5282, .T. ) ;
#12670 = EDGE_CURVE ( 'NONE', #13195, #3511, #1885, .T. ) ;
#12671 = ORIENTED_EDGE ( 'NONE', *, *, #7893, .F. ) ;
#12672 = CARTESIAN_POINT ( 'NONE',  ( -88.81638362644100937, 99.17411849586700612, -147.9984795835769944 ) ) ;
#12673 = ORIENTED_EDGE ( 'NONE', *, *, #14151, .T. ) ;
#12674 = VECTOR ( 'NONE', #14994, 1000.000000000000000 ) ;
#12675 = CARTESIAN_POINT ( 'NONE',  ( 4.172905853428635403, -0.9687499999999248379, 0.8311981373062848899 ) ) ;
#12676 = ORIENTED_EDGE ( 'NONE', *, *, #7793, .F. ) ;
#12677 = CARTESIAN_POINT ( 'NONE',  ( 3.525795616442236824, -2.921088562373113540, 1.882927806498691403 ) ) ;
#12678 = AXIS2_PLACEMENT_3D ( 'NONE', #3343, #5695, #11494 ) ;
#12679 = LINE ( 'NONE', #2053, #11189 ) ;
#12680 = CIRCLE ( 'NONE', #1540, 1.449999999999996403 ) ;
#12681 = CARTESIAN_POINT ( 'NONE',  ( -65.90140028023257912, 89.17411849586700612, -57.99847958357699440 ) ) ;
#12682 = CARTESIAN_POINT ( 'NONE',  ( 10.10406781373725771, -11.00000029085427045, 69.08979243323354069 ) ) ;
#12683 = VECTOR ( 'NONE', #3730, 1000.000000000000114 ) ;
#12684 = DIRECTION ( 'NONE',  ( -1.000000000000000000, 1.287488025362404182E-15, 0.000000000000000000 ) ) ;
#12685 = CARTESIAN_POINT ( 'NONE',  ( 4.573385150445044900, -3.618985300545107364, 6.000000000000001776 ) ) ;
#12686 = CARTESIAN_POINT ( 'NONE',  ( 2.598076211353309350, 2.375000000000006661, 4.500000000000000000 ) ) ;
#12687 = AXIS2_PLACEMENT_3D ( 'NONE', #13287, #166, #13135 ) ;
#12688 = PRODUCT_CONTEXT ( 'NONE', #11690, 'mechanical' ) ;
#12689 = ORIENTED_EDGE ( 'NONE', *, *, #6151, .F. ) ;
#12690 = CARTESIAN_POINT ( 'NONE',  ( -14.25000000000000000, -0.2038245569916330158, 21.77831216351300014 ) ) ;
#12691 = CARTESIAN_POINT ( 'NONE',  ( 3.567009421182318896, -4.953124999999990230, 1.083052099369142818 ) ) ;
#12692 = EDGE_LOOP ( 'NONE', ( #3592, #6079, #11858, #6901, #14255 ) ) ;
#12693 = AXIS2_PLACEMENT_3D ( 'NONE', #10697, #2470, #5353 ) ;
#12694 = CARTESIAN_POINT ( 'NONE',  ( -3.115386749435359093, -1.991250000000079678, -2.079980318098562098 ) ) ;
#12695 = DIRECTION ( 'NONE',  ( 0.000000000000000000, 1.000000000000000000, 0.000000000000000000 ) ) ;
#12696 = AXIS2_PLACEMENT_3D ( 'NONE', #3998, #11138, #13328 ) ;
#12697 = CARTESIAN_POINT ( 'NONE',  ( -15.50000000000000000, -0.1999999999999999556, 22.50000000000000000 ) ) ;
#12698 = CARTESIAN_POINT ( 'NONE',  ( 3.884135718427222717, -0.4995676945082492271, -1.024675529164014609 ) ) ;
#12699 = FACE_OUTER_BOUND ( 'NONE', #8704, .T. ) ;
#12700 = EDGE_CURVE ( 'NONE', #13871, #506, #1941, .T. ) ;
#12701 = PLANE ( 'NONE',  #9196 ) ;
#12702 = AXIS2_PLACEMENT_3D ( 'NONE', #4986, #3899, #12126 ) ;
#12703 = VERTEX_POINT ( 'NONE', #5374 ) ;
#12704 = CARTESIAN_POINT ( 'NONE',  ( -59.02799568714584666, 110.1741184958670061, -79.59847958357700293 ) ) ;
#12705 = ORIENTED_EDGE ( 'NONE', *, *, #5717, .T. ) ;
#12706 = ORIENTED_EDGE ( 'NONE', *, *, #45, .F. ) ;
#12707 = CARTESIAN_POINT ( 'NONE',  ( -3.313940955170608493, -4.131874999999921805, 1.004348227522814829 ) ) ;
#12708 = ORIENTED_EDGE ( 'NONE', *, *, #2499, .F. ) ;
#12709 = ORIENTED_EDGE ( 'NONE', *, *, #13695, .F. ) ;
#12710 = VECTOR ( 'NONE', #14846, 1000.000000000000000 ) ;
#12711 = AXIS2_PLACEMENT_3D ( 'NONE', #2096, #855, #11719 ) ;
#12712 = ORIENTED_EDGE ( 'NONE', *, *, #8062, .T. ) ;
#12713 = CARTESIAN_POINT ( 'NONE',  ( 6.573385150445030689, -19.31989681812820692, 0.000000000000000000 ) ) ;
#12714 = CARTESIAN_POINT ( 'NONE',  ( 1.148200974759891579, -0.3818749999999526135, 3.788695824010786861 ) ) ;
#12715 = AXIS2_PLACEMENT_3D ( 'NONE', #10955, #7403, #6468 ) ;
#12716 = CARTESIAN_POINT ( 'NONE',  ( -3.288344415138346744, -5.295814349376151142, 1.018963235593165262 ) ) ;
#12717 = DIRECTION ( 'NONE',  ( -0.000000000000000000, -0.000000000000000000, 1.000000000000000000 ) ) ;
#12718 = EDGE_CURVE ( 'NONE', #14870, #12409, #4197, .T. ) ;
#12719 = DIRECTION ( 'NONE',  ( 0.000000000000000000, 0.000000000000000000, 1.000000000000000000 ) ) ;
#12720 = CARTESIAN_POINT ( 'NONE',  ( 3.778928804394611873, 2.374507716408110092, 2.454703312603006005 ) ) ;
#12721 = CARTESIAN_POINT ( 'NONE',  ( -84.73238362643999722, 66.35306774555222376, -147.9984795835769944 ) ) ;
#12722 = LINE ( 'NONE', #5527, #15228 ) ;
#12723 = AXIS2_PLACEMENT_3D ( 'NONE', #13312, #7416, #14375 ) ;
#12724 = CARTESIAN_POINT ( 'NONE',  ( 17.12895037488186389, 3.654026927208769315, 0.2687305842673423095 ) ) ;
#12725 = EDGE_CURVE ( 'NONE', #5515, #2624, #3109, .T. ) ;
#12726 = CIRCLE ( 'NONE', #5556, 2.750000000000002665 ) ;
#12727 = CARTESIAN_POINT ( 'NONE',  ( 6.573385150445034242, -19.31989681812820692, 6.000000000000001776 ) ) ;
#12728 = EDGE_LOOP ( 'NONE', ( #2890, #1358, #707, #793, #4416, #2200 ) ) ;
#12729 = CARTESIAN_POINT ( 'NONE',  ( 15.50000000000000000, -1.037157890325000054, -26.00000000000000000 ) ) ;
#12730 = EDGE_LOOP ( 'NONE', ( #7460, #14497 ) ) ;
#12731 = VECTOR ( 'NONE', #2280, 1000.000000000000000 ) ;
#12732 = EDGE_LOOP ( 'NONE', ( #9881, #14802, #5977, #2965 ) ) ;
#12733 = VERTEX_POINT ( 'NONE', #14810 ) ;
#12734 = CYLINDRICAL_SURFACE ( 'NONE', #7501, 2.750000000000002665 ) ;
#12735 = CLOSED_SHELL ( 'NONE', ( #6795, #10056, #4219, #10554, #15284, #4459, #9208, #10294, #7654, #33, #12301, #11696, #898, #14815, #10757, #1491, #7039, #12816, #1199, #8462, #14524, #15027, #14080, #2687, #6889, #9414, #15297, #11990, #3836, #1084, #6984, #684, #809, #9635, #11516, #103, #4590, #9049, #3855, #6050, #11823, #9803, #9813, #5101, #14920, #108, #10088, #1186, #14542, #9867, #6759, #2808, #9233, #7277, #6668, #212, #5188, #12914, #7841, #12581, #7369, #963, #8446, #6891, #3704, #2958, #5934, #1066, #3464, #2212, #6148, #4873, #5364, #8390, #9882, #5231, #5007, #11118, #8395, #4310, #5390, #785, #565, #4039, #9063, #10763, #9433, #7471, #1578, #3621, #13620, #3927, #12022, #7846, #3934, #8669, #7525, #7694, #12576, #3057, #6990, #2984, #4915, #6948, #4561, #9983, #8124, #5847, #12203, #951, #9135, #4407, #501, #14464, #6605, #3161, #5543, #3075, #13877, #7799, #3671, #2319, #9145, #10935, #8819, #7235, #7732, #11443, #13399, #1547, #11705, #9106, #10462, #2434, #13543, #9111, #4989, #10880, #2243, #11711, #9617, #15262, #5157, #9519, #14727, #11147, #1367, #2868, #233, #9254, #10772, #9507, #6340, #1391, #7908, #4696, #12395, #6766, #5522, #7383, #3330, #11130, #12350, #15121, #313, #8408, #1383, #3364, #7573, #9794, #5969, #9230, #7324, #11218, #3043, #90, #11196, #13516, #3179, #11627, #14172, #11534, #12178, #1181, #1737, #5343, #14745, #13146, #11054, #11211, #2217, #11882, #7061, #9341, #1957, #11762, #7077, #9723, #6392, #7150, #3150, #4231, #7177, #4577, #2218, #1840, #13395, #12478, #3471, #9528, #5818 ) ) ;
#12736 = CARTESIAN_POINT ( 'NONE',  ( -2.189584623831577037, -4.225624999999936016, 2.666627758504775958 ) ) ;
#12737 = DIRECTION ( 'NONE',  ( -1.287488025362404182E-15, -1.000000000000000000, 0.000000000000000000 ) ) ;
#12738 = DIRECTION ( 'NONE',  ( -0.000000000000000000, -0.000000000000000000, -1.000000000000000000 ) ) ;
#12739 = CARTESIAN_POINT ( 'NONE',  ( 17.12895037488186389, -12.00000029085424025, 0.2687305842673423095 ) ) ;
#12740 = EDGE_CURVE ( 'NONE', #7739, #9509, #9074, .T. ) ;
#12741 = CARTESIAN_POINT ( 'NONE',  ( -53.77438362644000591, 82.17411849586700612, -183.7533135795160320 ) ) ;
#12742 = CARTESIAN_POINT ( 'NONE',  ( -63.06767964790545022, 68.65632084656354550, -83.44847958357698303 ) ) ;
#12743 = LINE ( 'NONE', #7009, #2067 ) ;
#12744 = CARTESIAN_POINT ( 'NONE',  ( -86.77438362644100778, 99.17411849586700612, -147.9984795835769944 ) ) ;
#12745 = EDGE_CURVE ( 'NONE', #8515, #6954, #5521, .T. ) ;
#12746 = ORIENTED_EDGE ( 'NONE', *, *, #14933, .F. ) ;
#12747 = FACE_OUTER_BOUND ( 'NONE', #6750, .T. ) ;
#12748 = VECTOR ( 'NONE', #4799, 1000.000000000000000 ) ;
#12749 = VECTOR ( 'NONE', #12628, 1000.000000000000000 ) ;
#12750 = ORIENTED_EDGE ( 'NONE', *, *, #5092, .T. ) ;
#12751 = EDGE_LOOP ( 'NONE', ( #12283, #3547, #1872, #4160 ) ) ;
#12752 = DIRECTION ( 'NONE',  ( -1.000000000000000000, 0.000000000000000000, 0.000000000000000000 ) ) ;
#12753 = VERTEX_POINT ( 'NONE', #7772 ) ;
#12754 = EDGE_CURVE ( 'NONE', #4229, #3116, #8375, .T. ) ;
#12755 = CARTESIAN_POINT ( 'NONE',  ( 2.374332146000840194, -0.8437500000000230926, 3.550666350934340354 ) ) ;
#12756 = VERTEX_POINT ( 'NONE', #14877 ) ;
#12757 = ADVANCED_FACE ( 'NONE', ( #7697 ), #7845, .F. ) ;
#12758 = CARTESIAN_POINT ( 'NONE',  ( -2.262274296814194230, -2.342963562372911923, -3.387670398104518199 ) ) ;
#12759 = DIRECTION ( 'NONE',  ( 1.000000000000000000, 0.000000000000000000, 0.000000000000000000 ) ) ;
#12760 = EDGE_CURVE ( 'NONE', #1550, #6145, #10216, .T. ) ;
#12761 = DIRECTION ( 'NONE',  ( 0.8660254037844485886, 0.000000000000000000, -0.4999999999999827360 ) ) ;
#12762 = CARTESIAN_POINT ( 'NONE',  ( -13.41835358098578723, 12.59999970914575940, -8.183940086454237317 ) ) ;
#12763 = AXIS2_PLACEMENT_3D ( 'NONE', #1716, #14511, #12192 ) ;
#12764 = EDGE_CURVE ( 'NONE', #9228, #12323, #1864, .T. ) ;
#12765 = CARTESIAN_POINT ( 'NONE',  ( -12.81835358098578403, 11.39999970914576366, -11.73358795631400397 ) ) ;
#12766 = EDGE_CURVE ( 'NONE', #4260, #5306, #2050, .T. ) ;
#12767 = DIRECTION ( 'NONE',  ( 0.000000000000000000, 0.000000000000000000, -1.000000000000000000 ) ) ;
#12768 = DIRECTION ( 'NONE',  ( 0.000000000000000000, 0.000000000000000000, 1.000000000000000000 ) ) ;
#12769 = ORIENTED_EDGE ( 'NONE', *, *, #10364, .F. ) ;
#12770 = AXIS2_PLACEMENT_3D ( 'NONE', #1365, #8058, #1285 ) ;
#12771 = CYLINDRICAL_SURFACE ( 'NONE', #13280, 0.6000000000000000888 ) ;
#12772 = CARTESIAN_POINT ( 'NONE',  ( 1.515516452534993119, -0.3975000000001072675, 3.655012690611889159 ) ) ;
#12773 = VERTEX_POINT ( 'NONE', #8773 ) ;
#12774 = AXIS2_PLACEMENT_3D ( 'NONE', #4406, #12484, #10131 ) ;
#12775 = CARTESIAN_POINT ( 'NONE',  ( -3.586083906644841779, -3.069375000000151399, -0.3518610084925551384 ) ) ;
#12776 = DIRECTION ( 'NONE',  ( 0.8660254037844387076, 0.4999999999999998890, 0.000000000000000000 ) ) ;
#12777 = CARTESIAN_POINT ( 'NONE',  ( 57.41329019055577021, 2.488961461112888074, 97.50956111919106206 ) ) ;
#12778 = VECTOR ( 'NONE', #241, 1000.000000000000000 ) ;
#12779 = DIRECTION ( 'NONE',  ( 1.000000000000000000, 1.541976423090494894E-16, 0.000000000000000000 ) ) ;
#12780 = AXIS2_PLACEMENT_3D ( 'NONE', #3067, #10114, #9176 ) ;
#12781 = DIRECTION ( 'NONE',  ( -0.000000000000000000, 1.000000000000000000, -0.000000000000000000 ) ) ;
#12782 = DIRECTION ( 'NONE',  ( 0.000000000000000000, 0.000000000000000000, 1.000000000000000000 ) ) ;
#12783 = AXIS2_PLACEMENT_3D ( 'NONE', #12231, #3700, #13172 ) ;
#12784 = CARTESIAN_POINT ( 'NONE',  ( -50.73238362644099197, 99.17411849586700612, -147.9984795835769944 ) ) ;
#12785 = ORIENTED_EDGE ( 'NONE', *, *, #12631, .T. ) ;
#12786 = CARTESIAN_POINT ( 'NONE',  ( 4.500000000000000888, 1.148368900306797357E-14, 0.000000000000000000 ) ) ;
#12787 = ORIENTED_EDGE ( 'NONE', *, *, #5065, .T. ) ;
#12788 = ORIENTED_EDGE ( 'NONE', *, *, #14094, .T. ) ;
#12789 = ORIENTED_EDGE ( 'NONE', *, *, #9724, .F. ) ;
#12790 = AXIS2_PLACEMENT_3D ( 'NONE', #4005, #513, #2692 ) ;
#12791 = VERTEX_POINT ( 'NONE', #11329 ) ;
#12792 = ORIENTED_EDGE ( 'NONE', *, *, #3653, .F. ) ;
#12793 = AXIS2_PLACEMENT_3D ( 'NONE', #9926, #7398, #5060 ) ;
#12794 = CARTESIAN_POINT ( 'NONE',  ( -2.502742494678076746, -6.374213562373193476, -2.504028389392794374 ) ) ;
#12795 = AXIS2_PLACEMENT_3D ( 'NONE', #4830, #15281, #10474 ) ;
#12796 = CARTESIAN_POINT ( 'NONE',  ( 3.915012698312653860, -0.5693749999999865308, 0.3866328316385073127 ) ) ;
#12797 = CARTESIAN_POINT ( 'NONE',  ( -0.4056240317154969355, -1.734374999999933831, 4.133709567805635920 ) ) ;
#12798 = DIRECTION ( 'NONE',  ( 0.003614861529251474706, 0.000000000000000000, -0.9999934663667180423 ) ) ;
#12799 = CARTESIAN_POINT ( 'NONE',  ( -4.463089466550673734, 2.239389106484332981, 1.269702285208761605 ) ) ;
#12800 = CYLINDRICAL_SURFACE ( 'NONE', #3924, 0.5999999999999998668 ) ;
#12801 = CARTESIAN_POINT ( 'NONE',  ( -52.77438362644000591, 65.17411849586700612, -152.4984795835769944 ) ) ;
#12802 = CIRCLE ( 'NONE', #11071, 3.968749999999992895 ) ;
#12803 = DIRECTION ( 'NONE',  ( -1.000000000000000000, 0.000000000000000000, 0.000000000000000000 ) ) ;
#12804 = DIRECTION ( 'NONE',  ( -1.000000000000000000, 0.000000000000000000, 0.000000000000000000 ) ) ;
#12805 = CARTESIAN_POINT ( 'NONE',  ( -12.81835358098578759, -12.00000029085424025, -8.733587956314007528 ) ) ;
#12806 = AXIS2_PLACEMENT_3D ( 'NONE', #8995, #12719, #10309 ) ;
#12807 = EDGE_LOOP ( 'NONE', ( #11893, #1090 ) ) ;
#12808 = CARTESIAN_POINT ( 'NONE',  ( 0.000000000000000000, 0.000000000000000000, -79.59847958357700293 ) ) ;
#12809 = ORIENTED_EDGE ( 'NONE', *, *, #6895, .F. ) ;
#12810 = VERTEX_POINT ( 'NONE', #11398 ) ;
#12811 = ORIENTED_EDGE ( 'NONE', *, *, #3832, .F. ) ;
#12812 = EDGE_CURVE ( 'NONE', #467, #2967, #1784, .T. ) ;
#12813 = CARTESIAN_POINT ( 'NONE',  ( 16.75000000000000000, -0.2038245569916320166, 23.22168783648699986 ) ) ;
#12814 = VECTOR ( 'NONE', #6248, 1000.000000000000000 ) ;
#12815 = CARTESIAN_POINT ( 'NONE',  ( -3.450064735799886595, -4.100625000000076348, 0.3410961574374171690 ) ) ;
#12816 = ADVANCED_FACE ( 'NONE', ( #10224 ), #12420, .F. ) ;
#12817 = AXIS2_PLACEMENT_3D ( 'NONE', #902, #15013, #4402 ) ;
#12818 = CARTESIAN_POINT ( 'NONE',  ( 15.08757311576526128, -0.3152598339554890106, 21.29473909965996015 ) ) ;
#12819 = CARTESIAN_POINT ( 'NONE',  ( -14.25000000000000000, -2.500000000000000000, -23.22168783648699986 ) ) ;
#12820 = CARTESIAN_POINT ( 'NONE',  ( 2.598076211353310239, 1.678847577293378857, -4.499999999999999112 ) ) ;
#12821 = CARTESIAN_POINT ( 'NONE',  ( -51.75338362643999801, 66.94254237039483257, -147.9984795835769944 ) ) ;
#12822 = CARTESIAN_POINT ( 'NONE',  ( -65.90140028023417074, 75.17411849586613926, -57.99847958357779021 ) ) ;
#12823 = CARTESIAN_POINT ( 'NONE',  ( -55.52438362644000591, 99.17411849586700612, -145.4984795835769660 ) ) ;
#12824 = CARTESIAN_POINT ( 'NONE',  ( -73.13733409597239188, 66.60412428008086749, -83.44847958357698303 ) ) ;
#12825 = DIRECTION ( 'NONE',  ( 0.000000000000000000, -1.000000000000000000, 0.000000000000000000 ) ) ;
#12826 = VERTEX_POINT ( 'NONE', #6391 ) ;
#12827 = DIRECTION ( 'NONE',  ( 2.551930889570659960E-15, -1.000000000000000000, -0.000000000000000000 ) ) ;
#12828 = ORIENTED_EDGE ( 'NONE', *, *, #1247, .F. ) ;
#12829 = CIRCLE ( 'NONE', #8120, 0.5999999999999999778 ) ;
#12830 = EDGE_LOOP ( 'NONE', ( #756, #10410, #8034, #6957 ) ) ;
#12831 = CYLINDRICAL_SURFACE ( 'NONE', #3258, 1.250000000000001110 ) ;
#12832 = ADVANCED_FACE ( 'NONE', ( #11104 ), #2881, .T. ) ;
#12833 = ITEM_DEFINED_TRANSFORMATION ( 'NONE', 'NONE', #13447,  #285 ) ;
#12834 = EDGE_CURVE ( 'NONE', #11758, #4603, #5034, .T. ) ;
#12835 = EDGE_LOOP ( 'NONE', ( #7101, #604 ) ) ;
#12836 = CARTESIAN_POINT ( 'NONE',  ( -3.579691249134443698, -0.5937499999999900080, 2.390491442833416080 ) ) ;
#12837 = ORIENTED_EDGE ( 'NONE', *, *, #2706, .T. ) ;
#12838 = CARTESIAN_POINT ( 'NONE',  ( -1.900756315137815067, -2.671088562373106434, 3.553810185735947869 ) ) ;
#12839 = LINE ( 'NONE', #13995, #12674 ) ;
#12840 = CARTESIAN_POINT ( 'NONE',  ( -69.77438362644001302, 82.17411849586700612, -67.69567958357700377 ) ) ;
#12841 = CIRCLE ( 'NONE', #11597, 16.06499999999999773 ) ;
#12842 = CARTESIAN_POINT ( 'NONE',  ( -52.77438362644000591, 65.17411849586700612, -86.49847958357699440 ) ) ;
#12843 = EDGE_CURVE ( 'NONE', #5278, #2560, #15184, .T. ) ;
#12844 = CARTESIAN_POINT ( 'NONE',  ( -104.2743836264399988, 60.67411849586700612, -79.49847958357700861 ) ) ;
#12845 = ORIENTED_EDGE ( 'NONE', *, *, #14163, .T. ) ;
#12846 = B_SPLINE_CURVE_WITH_KNOTS ( 'NONE', 3,
 ( #1647, #14666, #9931, #9699, #14590, #2728 ),
 .UNSPECIFIED., .F., .F.,
 ( 4, 2, 4 ),
 ( 1.820537833122030991, 2.555393473688635453, 3.290249114255240137 ),
 .UNSPECIFIED. ) ;
#12847 = PLANE ( 'NONE',  #9330 ) ;
#12848 = PLANE ( 'NONE',  #8976 ) ;
#12849 = ADVANCED_FACE ( 'NONE', ( #13955 ), #5751, .F. ) ;
#12850 = ORIENTED_EDGE ( 'NONE', *, *, #3312, .T. ) ;
#12851 = CARTESIAN_POINT ( 'NONE',  ( -3.686556889460768094, -0.1475000000000124822, 1.525885089196999056 ) ) ;
#12852 = EDGE_LOOP ( 'NONE', ( #14324, #1270 ) ) ;
#12853 = EDGE_CURVE ( 'NONE', #7763, #2194, #4729, .T. ) ;
#12854 = EDGE_CURVE ( 'NONE', #3303, #6571, #12216, .T. ) ;
#12855 = CARTESIAN_POINT ( 'NONE',  ( 0.7224497989600745518, -2.366250000000003517, 3.625028471221638071 ) ) ;
#12856 = CARTESIAN_POINT ( 'NONE',  ( -46.58670980944423690, 5.000000000000000000, 89.50956111919107627 ) ) ;
#12857 = DIRECTION ( 'NONE',  ( 0.000000000000000000, 1.000000000000000000, 0.000000000000000000 ) ) ;
#12858 = DIRECTION ( 'NONE',  ( -1.287488025362404182E-15, -1.000000000000000000, 0.000000000000000000 ) ) ;
#12859 = CIRCLE ( 'NONE', #4694, 4.499999999999997335 ) ;
#12860 = ADVANCED_FACE ( 'NONE', ( #996 ), #10453, .F. ) ;
#12861 = DIRECTION ( 'NONE',  ( -1.224646799147353207E-16, -2.139562256385042123E-31, 1.000000000000000000 ) ) ;
#12862 = DIRECTION ( 'NONE',  ( 0.000000000000000000, 0.000000000000000000, 1.000000000000000000 ) ) ;
#12863 = CARTESIAN_POINT ( 'NONE',  ( -15.50000000000000000, -1.037157890325000054, 18.50000000000000000 ) ) ;
#12864 = CARTESIAN_POINT ( 'NONE',  ( 15.50000000000000000, -2.500000000000000000, 23.94337567297399971 ) ) ;
#12865 = ORIENTED_EDGE ( 'NONE', *, *, #10564, .T. ) ;
#12866 = CARTESIAN_POINT ( 'NONE',  ( 57.41329019055577021, 2.488961461112888074, 95.72362361919107343 ) ) ;
#12867 = EDGE_CURVE ( 'NONE', #3023, #10723, #2237, .T. ) ;
#12868 = ORIENTED_EDGE ( 'NONE', *, *, #4556, .F. ) ;
#12869 = VERTEX_POINT ( 'NONE', #9215 ) ;
#12870 = CARTESIAN_POINT ( 'NONE',  ( -1.318845896519720506, -4.272500000000155396, 3.181678407182404467 ) ) ;
#12871 = VERTEX_POINT ( 'NONE', #11560 ) ;
#12872 = VERTEX_POINT ( 'NONE', #5685 ) ;
#12873 = ORIENTED_EDGE ( 'NONE', *, *, #13046, .T. ) ;
#12874 = CARTESIAN_POINT ( 'NONE',  ( 0.7191817349834368489, -5.217963562372981201, -3.622537723569287493 ) ) ;
#12875 = B_SPLINE_CURVE_WITH_KNOTS ( 'NONE', 3,
 ( #1082, #5402, #13614, #9380, #10170, #5471, #10460, #7868, #3134, #3487, #3413, #10543, #12444, #13684, #13760, #567, #2244, #6989, #4294, #3054, #12375, #15270, #1733, #4579, #5316, #2981, #12602, #9304, #14044, #14117, #12526, #6483, #9019, #6714, #11426, #14766, #4664, #1002, #8150, #12884, #11716, #11197, #10030, #4152, #8875, #1807, #9527, #1234, #4967, #8447, #2473, #2552, #11794, #1162, #2402, #2325, #8382, #10699, #7302, #3718, #67, #6157, #9676, #9450, #13123, #12963, #8667, #4818, #5921, #7073, #9605, #12030, #4734, #10622, #14270, #14189, #1399, #222, #10864, #3569, #148, #13192, #7221, #14410, #3649, #5994, #3796, #8303, #11944, #8527, #13044, #1311, #13273, #6075, #14340, #8223, #7151, #10786, #11872, #4900, #2145, #12775, #7956, #8271, #13012, #3460, #1132, #14012, #3388, #5658, #3226, #8190, #4635, #8038, #1049, #4548, #9353, #900, #9273, #10357, #13933, #15083, #3536, #4470, #9190, #974, #10280, #15009, #3304, #8121, #5893, #12855, #6892, #11610, #10595, #5727, #10429, #4709, #14093, #2215, #12928, #15158, #6958, #11680, #5805, #6736, #9421, #12694, #10511, #14160, #11764, #15317, #2066, #15239, #11456, #6816, #2290, #4400, #821, #7040, #5579, #9119, #13858, #11535, #14237, #10986, #13243, #6273, #3925, #7429, #9732, #10834, #13324, #6126, #14317, #5016, #8357, #3695, #8649, #7198, #14383, #2684, #12147, #10752, #8424, #2604, #4782, #7352, #4942, #9499, #13166, #3622, #2371, #7123, #14468, #1517, #9650, #3770, #1282, #13098, #3852, #2448, #11919, #6047, #196, #2523, #352, #8499, #5100, #11999, #117, #14543, #4868, #12080 ),
 .UNSPECIFIED., .F., .F.,
 ( 4, 2, 2, 2, 2, 2, 2, 2, 2, 2, 2, 2, 2, 2, 2, 2, 2, 2, 2, 2, 2, 2, 2, 2, 2, 2, 2, 2, 2, 2, 2, 2, 2, 2, 2, 2, 2, 2, 2, 2, 2, 2, 2, 2, 2, 2, 2, 2, 2, 2, 2, 2, 2, 2, 2, 2, 2, 2, 2, 2, 2, 2, 2, 2, 2, 2, 2, 2, 2, 2, 2, 2, 2, 2, 2, 2, 2, 2, 2, 2, 2, 2, 2, 2, 2, 2, 2, 2, 2, 2, 2, 2, 2, 2, 2, 2, 2, 2, 2, 2, 2, 2, 2, 2, 2, 2, 4 ),
 ( 0.1106917040526264190, 0.1171875000000000000, 0.1250000000000000000, 0.1328125000000000000, 0.1406250000000000000, 0.1484375000000000000, 0.1562500000000000000, 0.1640625000000000000, 0.1718750000000000000, 0.1796875000000000000, 0.1875000000000000000, 0.1953125000000000000, 0.2031250000000000000, 0.2109375000000000000, 0.2187500000000000000, 0.2265625000000000000, 0.2343750000000000000, 0.2421875000000000000, 0.2500000000000000000, 0.2578125000000000000, 0.2656250000000000000, 0.2734375000000000000, 0.2812500000000000000, 0.2890625000000000000, 0.2968750000000000000, 0.3046875000000000000, 0.3125000000000000000, 0.3203125000000000555, 0.3281250000000000000, 0.3359375000000000000, 0.3437500000000000000, 0.3515625000000000000, 0.3593750000000000000, 0.3671875000000000000, 0.3750000000000000000, 0.3828125000000000000, 0.3906250000000000000, 0.3984375000000000000, 0.4062500000000000000, 0.4140625000000000000, 0.4218750000000000000, 0.4296875000000000000, 0.4374999999999999445, 0.4453125000000000000, 0.4531250000000000000, 0.4609375000000000000, 0.4687500000000000000, 0.4765625000000000555, 0.4843750000000000000, 0.4921875000000000000, 0.5000000000000000000, 0.5078125000000000000, 0.5156250000000000000, 0.5234375000000000000, 0.5312500000000000000, 0.5390625000000000000, 0.5468750000000000000, 0.5546875000000000000, 0.5625000000000000000, 0.5703125000000000000, 0.5781250000000000000, 0.5859375000000000000, 0.5937500000000000000, 0.6015625000000001110, 0.6093750000000000000, 0.6171875000000000000, 0.6250000000000000000, 0.6328125000000000000, 0.6406250000000000000, 0.6484375000000000000, 0.6562500000000000000, 0.6640625000000000000, 0.6718750000000000000, 0.6796875000000000000, 0.6875000000000000000, 0.6953125000000000000, 0.7031250000000000000, 0.7109375000000000000, 0.7187500000000000000, 0.7265625000000000000, 0.7343750000000000000, 0.7421875000000000000, 0.7499999999999998890, 0.7578125000000000000, 0.7656250000000000000, 0.7734375000000000000, 0.7812500000000000000, 0.7890625000000001110, 0.7968750000000000000, 0.8046875000000000000, 0.8125000000000000000, 0.8203125000000000000, 0.8281250000000001110, 0.8359375000000000000, 0.8437500000000000000, 0.8515625000000000000, 0.8593750000000000000, 0.8671875000000001110, 0.8750000000000000000, 0.8828125000000000000, 0.8906250000000000000, 0.8984375000000000000, 0.9062500000000000000, 0.9140625000000000000, 0.9218749999999998890, 0.9296875000000000000, 0.9309053842486232355 ),
 .UNSPECIFIED. ) ;
#12876 = DIRECTION ( 'NONE',  ( -1.000000000000000000, 0.000000000000000000, 0.000000000000000000 ) ) ;
#12877 = LINE ( 'NONE', #8439, #8097 ) ;
#12878 = CARTESIAN_POINT ( 'NONE',  ( -88.81638362644100937, 100.3530677455522238, -147.9984795835769944 ) ) ;
#12879 = CARTESIAN_POINT ( 'NONE',  ( -56.85838362644099675, 99.17411849586700612, -147.9984795835769944 ) ) ;
#12880 = CARTESIAN_POINT ( 'NONE',  ( -69.77438362644001302, 90.17411849586700612, -29.37106258560738681 ) ) ;
#12881 = FACE_OUTER_BOUND ( 'NONE', #3724, .T. ) ;
#12882 = DIRECTION ( 'NONE',  ( 0.000000000000000000, 1.000000000000000000, 0.000000000000000000 ) ) ;
#12883 = CARTESIAN_POINT ( 'NONE',  ( 16.75000000000000000, -0.2038245569916320166, -21.77831216351300014 ) ) ;
#12884 = CARTESIAN_POINT ( 'NONE',  ( 3.151910583997929116, -4.522499999999531894, 1.304188709559700232 ) ) ;
#12885 = DIRECTION ( 'NONE',  ( 0.000000000000000000, 0.000000000000000000, -1.000000000000000000 ) ) ;
#12886 = ORIENTED_EDGE ( 'NONE', *, *, #11974, .T. ) ;
#12887 = DIRECTION ( 'NONE',  ( -1.000000000000000000, 0.000000000000000000, 0.000000000000000000 ) ) ;
#12888 = ORIENTED_EDGE ( 'NONE', *, *, #14316, .F. ) ;
#12889 = EDGE_LOOP ( 'NONE', ( #1703, #6064, #835, #1631 ) ) ;
#12890 = FACE_OUTER_BOUND ( 'NONE', #1257, .T. ) ;
#12891 = CARTESIAN_POINT ( 'NONE',  ( -91.02438362643999881, 65.17411849586700612, -182.2484795835770228 ) ) ;
#12892 = CARTESIAN_POINT ( 'NONE',  ( 57.41329019055577021, 5.000000000000001776, 101.4783111191910621 ) ) ;
#12893 = DIRECTION ( 'NONE',  ( 0.000000000000000000, 0.000000000000000000, -1.000000000000000000 ) ) ;
#12894 = FACE_OUTER_BOUND ( 'NONE', #10508, .T. ) ;
#12895 = CARTESIAN_POINT ( 'NONE',  ( -70.45539183192644828, 89.17411849586699191, -44.02377680093030676 ) ) ;
#12896 = FACE_OUTER_BOUND ( 'NONE', #6529, .T. ) ;
#12897 = CARTESIAN_POINT ( 'NONE',  ( -63.28565528768381654, 67.29799558322736175, -83.44847958357698303 ) ) ;
#12898 = ORIENTED_EDGE ( 'NONE', *, *, #12485, .T. ) ;
#12899 = CARTESIAN_POINT ( 'NONE',  ( -53.27438362644000591, 82.17411849586700612, -150.4984795835769944 ) ) ;
#12900 = EDGE_CURVE ( 'NONE', #14841, #14332, #802, .T. ) ;
#12901 = ORIENTED_EDGE ( 'NONE', *, *, #2989, .T. ) ;
#12902 = ORIENTED_EDGE ( 'NONE', *, *, #10785, .T. ) ;
#12903 = CARTESIAN_POINT ( 'NONE',  ( -16.75000000000000000, -2.500000000000000000, 21.77831216351300014 ) ) ;
#12904 = ORIENTED_EDGE ( 'NONE', *, *, #2580, .T. ) ;
#12905 = CARTESIAN_POINT ( 'NONE',  ( 1.227202584385329587, -1.203124999999989342, -4.041673972266214498 ) ) ;
#12906 = EDGE_LOOP ( 'NONE', ( #9384, #227, #12397, #10339 ) ) ;
#12907 = CARTESIAN_POINT ( 'NONE',  ( -0.7695070984847973694, -3.280463562373082009, -3.873892029236536416 ) ) ;
#12908 = AXIS2_PLACEMENT_3D ( 'NONE', #4080, #6354, #14844 ) ;
#12909 = LINE ( 'NONE', #5562, #10686 ) ;
#12910 = DIRECTION ( 'NONE',  ( 0.000000000000000000, 0.000000000000000000, 1.000000000000000000 ) ) ;
#12911 = VECTOR ( 'NONE', #4471, 1000.000000000000000 ) ;
#12912 = DIRECTION ( 'NONE',  ( -1.000000000000000000, 0.000000000000000000, -0.000000000000000000 ) ) ;
#12913 = PRODUCT_RELATED_PRODUCT_CATEGORY ( 'part', '', ( #2385 ) ) ;
#12914 = ADVANCED_FACE ( 'NONE', ( #13880 ), #6983, .T. ) ;
#12915 = PRODUCT ( 'Part1', 'Part1', '', ( #3614 ) ) ;
#12916 = DIRECTION ( 'NONE',  ( -1.000000000000000000, 0.000000000000000000, 0.000000000000000000 ) ) ;
#12917 = VERTEX_POINT ( 'NONE', #924 ) ;
#12918 = CARTESIAN_POINT ( 'NONE',  ( 4.573385150445044900, -3.618985300545107364, 6.000000000000000000 ) ) ;
#12919 = EDGE_CURVE ( 'NONE', #4529, #9060, #5542, .T. ) ;
#12920 = CARTESIAN_POINT ( 'NONE',  ( -15.50000000000000000, 998.9628421096749662, -22.50000000000000000 ) ) ;
#12921 = AXIS2_PLACEMENT_3D ( 'NONE', #1116, #11663, #11595 ) ;
#12922 = SHAPE_DEFINITION_REPRESENTATION ( #14743, #11263 ) ;
#12923 = ORIENTED_EDGE ( 'NONE', *, *, #8677, .F. ) ;
#12924 = AXIS2_PLACEMENT_3D ( 'NONE', #11746, #5870, #1113 ) ;
#12925 = CARTESIAN_POINT ( 'NONE',  ( 23.25000000000000000, -5.000000000000000000, 0.000000000000000000 ) ) ;
#12926 = CARTESIAN_POINT ( 'NONE',  ( 3.049996619588438040, -0.4756250000000030176, 2.504408566260782010 ) ) ;
#12927 = VERTEX_POINT ( 'NONE', #14356 ) ;
#12928 = CARTESIAN_POINT ( 'NONE',  ( -3.284049251726958829, -2.163124999999908482, 1.754264853118110423 ) ) ;
#12929 = DIRECTION ( 'NONE',  ( 0.000000000000000000, 0.000000000000000000, 1.000000000000000000 ) ) ;
#12930 = CIRCLE ( 'NONE', #6265, 2.750000000000002665 ) ;
#12931 = DIRECTION ( 'NONE',  ( -1.000000000000000000, -1.747085166004344019E-15, 0.000000000000000000 ) ) ;
#12932 = EDGE_CURVE ( 'NONE', #2624, #6663, #6531, .T. ) ;
#12933 = LINE ( 'NONE', #2295, #13001 ) ;
#12934 = AXIS2_PLACEMENT_3D ( 'NONE', #4743, #1320, #4672 ) ;
#12935 = CARTESIAN_POINT ( 'NONE',  ( 21.98164641901421135, -12.00000029085424202, -0.3335879563140091153 ) ) ;
#12936 = FILL_AREA_STYLE_COLOUR ( '', #1297 ) ;
#12937 = AXIS2_PLACEMENT_3D ( 'NONE', #15090, #15164, #6899 ) ;
#12938 = EDGE_CURVE ( 'NONE', #1333, #6768, #15160, .T. ) ;
#12939 = DIRECTION ( 'NONE',  ( 2.551930889570659960E-15, -1.000000000000000000, -0.000000000000000000 ) ) ;
#12940 = EDGE_CURVE ( 'NONE', #1111, #8072, #6758, .T. ) ;
#12941 = ORIENTED_EDGE ( 'NONE', *, *, #10364, .T. ) ;
#12942 = DIRECTION ( 'NONE',  ( -1.000000000000000000, 0.000000000000000000, 0.000000000000000000 ) ) ;
#12943 = VERTEX_POINT ( 'NONE', #4657 ) ;
#12944 = TOROIDAL_SURFACE ( 'NONE', #7748, -1.151041666666720031, 4.401041666666736241 ) ;
#12945 = VERTEX_POINT ( 'NONE', #2164 ) ;
#12946 = CARTESIAN_POINT ( 'NONE',  ( 0.6569748927284411177, -4.803749999999888054, -3.309289439050847381 ) ) ;
#12947 = ORIENTED_EDGE ( 'NONE', *, *, #12172, .F. ) ;
#12948 = VERTEX_POINT ( 'NONE', #2317 ) ;
#12949 = ORIENTED_EDGE ( 'NONE', *, *, #3736, .F. ) ;
#12950 = PRODUCT_DEFINITION_FORMATION_WITH_SPECIFIED_SOURCE ( 'ANY', '', #1739, .NOT_KNOWN. ) ;
#12951 = CARTESIAN_POINT ( 'NONE',  ( 3.837897214521031053, -3.983588562373158837, 0.3790132011682106339 ) ) ;
#12952 = EDGE_CURVE ( 'NONE', #10071, #11036, #8493, .T. ) ;
#12953 = AXIS2_PLACEMENT_3D ( 'NONE', #7192, #1357, #11912 ) ;
#12954 = DIRECTION ( 'NONE',  ( -1.000000000000000000, 0.000000000000000000, 0.000000000000000000 ) ) ;
#12955 = DIRECTION ( 'NONE',  ( 0.000000000000000000, 0.000000000000000000, 1.000000000000000000 ) ) ;
#12956 = CARTESIAN_POINT ( 'NONE',  ( 3.584540577507836603E-16, 9.015594676761164550, 0.000000000000000000 ) ) ;
#12957 = EDGE_CURVE ( 'NONE', #11895, #13217, #14111, .T. ) ;
#12958 = FACE_OUTER_BOUND ( 'NONE', #7440, .T. ) ;
#12959 = AXIS2_PLACEMENT_3D ( 'NONE', #13351, #6223, #1473 ) ;
#12960 = CARTESIAN_POINT ( 'NONE',  ( -62.27438362644000591, 75.17411849586699191, -57.99847958357699440 ) ) ;
#12961 = DIRECTION ( 'NONE',  ( 0.000000000000000000, 0.000000000000000000, 1.000000000000000000 ) ) ;
#12962 = DIRECTION ( 'NONE',  ( -1.000000000000000000, 0.000000000000000000, 0.000000000000000000 ) ) ;
#12963 = CARTESIAN_POINT ( 'NONE',  ( -1.647113530155736916, -3.913124999999971099, -3.078783428963292490 ) ) ;
#12964 = EDGE_CURVE ( 'NONE', #3958, #3363, #5988, .T. ) ;
#12965 = FACE_OUTER_BOUND ( 'NONE', #7176, .T. ) ;
#12966 = ADVANCED_FACE ( 'NONE', ( #12225 ), #3856, .F. ) ;
#12967 = ORIENTED_EDGE ( 'NONE', *, *, #6703, .T. ) ;
#12968 = DIRECTION ( 'NONE',  ( 0.000000000000000000, 0.000000000000000000, -1.000000000000000000 ) ) ;
#12969 = AXIS2_PLACEMENT_3D ( 'NONE', #13591, #696, #4266 ) ;
#12970 = VERTEX_POINT ( 'NONE', #2755 ) ;
#12971 = ORIENTED_EDGE ( 'NONE', *, *, #6853, .T. ) ;
#12972 = ORIENTED_EDGE ( 'NONE', *, *, #4317, .F. ) ;
#12973 = AXIS2_PLACEMENT_3D ( 'NONE', #86, #4838, #7241 ) ;
#12974 =( NAMED_UNIT ( * ) PLANE_ANGLE_UNIT ( ) SI_UNIT ( $, .RADIAN. ) );
#12975 = CARTESIAN_POINT ( 'NONE',  ( 1.342127543875233808, -3.772500000000060805, -3.243584335895732362 ) ) ;
#12976 = CARTESIAN_POINT ( 'NONE',  ( 14.25000000000000000, -0.2038245569916330158, 21.77831216351300014 ) ) ;
#12977 = CARTESIAN_POINT ( 'NONE',  ( 1.432789758436758154, -4.812499999999716671, 3.461605376534508505 ) ) ;
#12978 = AXIS2_PLACEMENT_3D ( 'NONE', #7650, #12374, #2825 ) ;
#12979 = CARTESIAN_POINT ( 'NONE',  ( 1.555132164100668124, 2.118440305064532403, -4.499999999999999112 ) ) ;
#12980 = VECTOR ( 'NONE', #4719, 1000.000000000000000 ) ;
#12981 = CARTESIAN_POINT ( 'NONE',  ( -23.25000000000000000, -10.00000000000000000, -27.00000000000000000 ) ) ;
#12982 = DIRECTION ( 'NONE',  ( 9.422394424380278809E-16, -1.000000000000000000, 0.000000000000000000 ) ) ;
#12983 = DIRECTION ( 'NONE',  ( -1.000000000000000000, -0.000000000000000000, -0.000000000000000000 ) ) ;
#12984 = DIRECTION ( 'NONE',  ( 0.9999934663667179313, 0.000000000000000000, 0.003614861529252313445 ) ) ;
#12985 = LINE ( 'NONE', #11653, #13463 ) ;
#12986 = AXIS2_PLACEMENT_3D ( 'NONE', #14513, #8468, #5219 ) ;
#12987 = EDGE_LOOP ( 'NONE', ( #12109, #211 ) ) ;
#12988 = CARTESIAN_POINT ( 'NONE',  ( -69.77438362644100778, 82.17411849586700612, -79.49847958357700861 ) ) ;
#12989 = EDGE_LOOP ( 'NONE', ( #9345, #3314, #2073, #10940 ) ) ;
#12990 = ORIENTED_EDGE ( 'NONE', *, *, #10949, .T. ) ;
#12991 = CARTESIAN_POINT ( 'NONE',  ( 17.18164641901421419, -12.00000029085424025, 0.8664120436859875651 ) ) ;
#12992 = AXIS2_PLACEMENT_3D ( 'NONE', #6481, #11194, #14764 ) ;
#12993 = CONICAL_SURFACE ( 'NONE', #14710, 8.349999999999996092, 0.7853981633974476129 ) ;
#12994 = CARTESIAN_POINT ( 'NONE',  ( 4.056584590913882238, 0.06249999999998995942, 1.681565391176998769 ) ) ;
#12995 = ORIENTED_EDGE ( 'NONE', *, *, #11774, .F. ) ;
#12996 = CARTESIAN_POINT ( 'NONE',  ( 4.061877285462823117, -1.046088562372976982, -1.233758211555065154 ) ) ;
#12997 = FACE_OUTER_BOUND ( 'NONE', #1652, .T. ) ;
#12998 = DIRECTION ( 'NONE',  ( 0.000000000000000000, 0.000000000000000000, 1.000000000000000000 ) ) ;
#12999 = CARTESIAN_POINT ( 'NONE',  ( -69.77438362644001302, 82.17411849586700612, -152.4984795835769944 ) ) ;
#13000 = VECTOR ( 'NONE', #11937, 1000.000000000000000 ) ;
#13001 = VECTOR ( 'NONE', #7046, 1000.000000000000000 ) ;
#13002 = DIRECTION ( 'NONE',  ( 0.000000000000000000, -0.000000000000000000, 1.000000000000000000 ) ) ;
#13003 = ORIENTED_EDGE ( 'NONE', *, *, #886, .T. ) ;
#13004 = DIRECTION ( 'NONE',  ( -0.1305261922200569580, 0.9914448613738096050, 0.000000000000000000 ) ) ;
#13005 = DIRECTION ( 'NONE',  ( -0.8660254037844387076, -2.210036979070413080E-15, -0.4999999999999998890 ) ) ;
#13006 = ORIENTED_EDGE ( 'NONE', *, *, #13072, .T. ) ;
#13007 = DIRECTION ( 'NONE',  ( 1.049727191138615614E-16, 0.8571673007021106683, 0.5150380749100569311 ) ) ;
#13008 = CARTESIAN_POINT ( 'NONE',  ( -0.3822054598150002591, -3.734374999999974243, 3.870204888229129114 ) ) ;
#13009 = ORIENTED_EDGE ( 'NONE', *, *, #8409, .T. ) ;
#13010 = EDGE_CURVE ( 'NONE', #6866, #4383, #8581, .T. ) ;
#13011 = VECTOR ( 'NONE', #10458, 1000.000000000000114 ) ;
#13012 = CARTESIAN_POINT ( 'NONE',  ( -3.184718056276182097, -3.006875000000130083, -1.703323619722481475 ) ) ;
#13013 = DIRECTION ( 'NONE',  ( 0.000000000000000000, 0.000000000000000000, -1.000000000000000000 ) ) ;
#13014 = EDGE_CURVE ( 'NONE', #5785, #4566, #5178, .T. ) ;
#13015 = DIRECTION ( 'NONE',  ( 0.000000000000000000, 0.000000000000000000, -1.000000000000000000 ) ) ;
#13016 = DIRECTION ( 'NONE',  ( 0.000000000000000000, 0.000000000000000000, -1.000000000000000000 ) ) ;
#13017 = DIRECTION ( 'NONE',  ( -0.000000000000000000, -0.000000000000000000, 1.000000000000000000 ) ) ;
#13018 = DIRECTION ( 'NONE',  ( -1.000000000000000000, -2.622621077317916910E-15, 0.000000000000000000 ) ) ;
#13019 = LINE ( 'NONE', #10841, #3044 ) ;
#13020 = CARTESIAN_POINT ( 'NONE',  ( 40.52020888806953991, 0.000000000000000000, 0.000000000000000000 ) ) ;
#13021 = DIRECTION ( 'NONE',  ( 1.000000000000000000, 0.000000000000000000, 0.000000000000000000 ) ) ;
#13022 = AXIS2_PLACEMENT_3D ( 'NONE', #5600, #1861, #12418 ) ;
#13023 = EDGE_LOOP ( 'NONE', ( #10341, #12828, #15332, #15197, #991 ) ) ;
#13024 = CIRCLE ( 'NONE', #2617, 4.000000000000000000 ) ;
#13025 = DIRECTION ( 'NONE',  ( 1.000000000000000000, 0.000000000000000000, -0.000000000000000000 ) ) ;
#13026 = ORIENTED_EDGE ( 'NONE', *, *, #11496, .F. ) ;
#13027 = CARTESIAN_POINT ( 'NONE',  ( -52.77438362644000591, 99.17411849586700612, -145.4984795835769660 ) ) ;
#13028 = CARTESIAN_POINT ( 'NONE',  ( -2.894177851434075688, -3.991249999999941789, -1.934899151906828374 ) ) ;
#13029 = ORIENTED_EDGE ( 'NONE', *, *, #1242, .F. ) ;
#13030 = ORIENTED_EDGE ( 'NONE', *, *, #11728, .F. ) ;
#13031 = EDGE_CURVE ( 'NONE', #1927, #4923, #63, .T. ) ;
#13032 = ORIENTED_EDGE ( 'NONE', *, *, #7928, .F. ) ;
#13033 = CARTESIAN_POINT ( 'NONE',  ( 3.854459931122866223, -3.999213562372995856, -0.001409750848530770366 ) ) ;
#13034 = AXIS2_PLACEMENT_3D ( 'NONE', #504, #2917, #12381 ) ;
#13035 = DIRECTION ( 'NONE',  ( 0.000000000000000000, 0.000000000000000000, 1.000000000000000000 ) ) ;
#13036 = EDGE_CURVE ( 'NONE', #14943, #8436, #10720, .T. ) ;
#13037 = AXIS2_PLACEMENT_3D ( 'NONE', #11982, #9484, #9640 ) ;
#13038 = VECTOR ( 'NONE', #3648, 1000.000000000000000 ) ;
#13039 = CARTESIAN_POINT ( 'NONE',  ( -3.012508034349790975, 2.058119353682387409, 3.782183026296721540 ) ) ;
#13040 = DIRECTION ( 'NONE',  ( 2.551930889570659960E-15, -1.000000000000000000, -0.000000000000000000 ) ) ;
#13041 = LINE ( 'NONE', #4495, #7617 ) ;
#13042 = DIRECTION ( 'NONE',  ( -0.7071067811865474617, 0.000000000000000000, -0.7071067811865474617 ) ) ;
#13043 = CARTESIAN_POINT ( 'NONE',  ( 57.41329019055577021, 5.000000000000001776, 97.50956111919106206 ) ) ;
#13044 = CARTESIAN_POINT ( 'NONE',  ( -0.0009180086920793713474, -3.334999999999859632, 3.568205616840286698 ) ) ;
#13045 = CARTESIAN_POINT ( 'NONE',  ( 40.52020888806953991, 0.000000000000000000, 6.000000000000000000 ) ) ;
#13046 = EDGE_CURVE ( 'NONE', #3023, #10251, #7020, .T. ) ;
#13047 = VERTEX_POINT ( 'NONE', #1745 ) ;
#13048 = EDGE_CURVE ( 'NONE', #4095, #11284, #11459, .T. ) ;
#13049 = FACE_OUTER_BOUND ( 'NONE', #10793, .T. ) ;
#13050 = AXIS2_PLACEMENT_3D ( 'NONE', #11637, #1001, #8149 ) ;
#13051 = EDGE_LOOP ( 'NONE', ( #3321, #7366, #15136, #2350 ) ) ;
#13052 = CIRCLE ( 'NONE', #11074, 4.500000000000000888 ) ;
#13053 = VERTEX_POINT ( 'NONE', #3928 ) ;
#13054 = ORIENTED_EDGE ( 'NONE', *, *, #11903, .F. ) ;
#13055 = AXIS2_PLACEMENT_3D ( 'NONE', #9638, #10967, #13225 ) ;
#13056 = EDGE_CURVE ( 'NONE', #13261, #8742, #14546, .T. ) ;
#13057 = CARTESIAN_POINT ( 'NONE',  ( -37.27438362644000591, 99.17411849586700612, -15.85886927678779834 ) ) ;
#13058 = CARTESIAN_POINT ( 'NONE',  ( 1.033118776976089670, -3.381875000000070131, 3.408891928937246796 ) ) ;
#13059 = EDGE_CURVE ( 'NONE', #8152, #9489, #8651, .T. ) ;
#13060 = PRODUCT_DEFINITION_SHAPE ( 'NONE', 'NONE',  #13774 ) ;
#13061 = EDGE_CURVE ( 'NONE', #4503, #2194, #13459, .T. ) ;
#13062 = CARTESIAN_POINT ( 'NONE',  ( -42.77438362644000591, 110.1741184958670061, -15.85886927678779834 ) ) ;
#13063 = VECTOR ( 'NONE', #11282, 1000.000000000000114 ) ;
#13064 = CARTESIAN_POINT ( 'NONE',  ( 15.50000000000000000, -5.000000000000000000, -22.50000000000000000 ) ) ;
#13065 = CARTESIAN_POINT ( 'NONE',  ( 0.9018160986354060160, 2.304554878306184218, -4.499999999999999112 ) ) ;
#13066 = DIRECTION ( 'NONE',  ( 0.000000000000000000, 1.000000000000000000, 0.000000000000000000 ) ) ;
#13067 = CARTESIAN_POINT ( 'NONE',  ( -16.33757311576526305, -0.3152598339554828488, 23.45980260912095616 ) ) ;
#13068 = CARTESIAN_POINT ( 'NONE',  ( -71.12250604111588359, 89.17411849586699191, -44.11946707556861469 ) ) ;
#13069 = LINE ( 'NONE', #1251, #2103 ) ;
#13070 = CARTESIAN_POINT ( 'NONE',  ( -15.29686605391142606, -0.2715358723588626733, -21.17390376548178210 ) ) ;
#13071 = CARTESIAN_POINT ( 'NONE',  ( -72.92551479769302603, 97.86074886511958937, -93.49847958357699440 ) ) ;
#13072 = EDGE_CURVE ( 'NONE', #5033, #5785, #13560, .T. ) ;
#13073 = ORIENTED_EDGE ( 'NONE', *, *, #10178, .F. ) ;
#13074 = DIRECTION ( 'NONE',  ( 0.000000000000000000, 0.000000000000000000, -1.000000000000000000 ) ) ;
#13075 = ORIENTED_EDGE ( 'NONE', *, *, #6637, .F. ) ;
#13076 = EDGE_LOOP ( 'NONE', ( #1950, #6790, #4483, #8423 ) ) ;
#13077 = ORIENTED_EDGE ( 'NONE', *, *, #9146, .F. ) ;
#13078 = DIRECTION ( 'NONE',  ( -1.000000000000000000, 0.000000000000000000, 0.000000000000000000 ) ) ;
#13079 = AXIS2_PLACEMENT_3D ( 'NONE', #9097, #14838, #6485 ) ;
#13080 = EDGE_CURVE ( 'NONE', #6471, #8682, #12150, .T. ) ;
#13081 = CARTESIAN_POINT ( 'NONE',  ( -0.001183910938090454099, 0.2499999999998853417, 4.416106207682124918 ) ) ;
#13082 = VERTEX_POINT ( 'NONE', #11210 ) ;
#13083 = CARTESIAN_POINT ( 'NONE',  ( 1.204928114531795158, -1.796088562373254982, 3.966944375248610655 ) ) ;
#13084 = DIRECTION ( 'NONE',  ( 0.3479852726768751237, 0.000000000000000000, -0.9375000000000004441 ) ) ;
#13085 = CARTESIAN_POINT ( 'NONE',  ( -65.90140028023417074, 75.17411849586613926, -57.99847958357779021 ) ) ;
#13086 = LINE ( 'NONE', #3607, #4541 ) ;
#13087 = AXIS2_PLACEMENT_3D ( 'NONE', #8085, #15207, #9394 ) ;
#13088 = CARTESIAN_POINT ( 'NONE',  ( -86.77438362644001302, 82.17411849586700612, -79.59847958357700293 ) ) ;
#13089 = ORIENTED_EDGE ( 'NONE', *, *, #8192, .F. ) ;
#13090 = LINE ( 'NONE', #3451, #7372 ) ;
#13091 = CARTESIAN_POINT ( 'NONE',  ( -35.27438362644000591, 72.17411849586700612, -67.49847958357700861 ) ) ;
#13092 = SHAPE_DEFINITION_REPRESENTATION ( #626, #2929 ) ;
#13093 = EDGE_LOOP ( 'NONE', ( #6054, #1302, #2789, #5322, #10501, #14104 ) ) ;
#13094 =( NAMED_UNIT ( * ) SI_UNIT ( $, .STERADIAN. ) SOLID_ANGLE_UNIT ( ) );
#13095 = CARTESIAN_POINT ( 'NONE',  ( -3.506684959068008034, -4.437500000000057732, -1.453587443624275499 ) ) ;
#13096 = EDGE_LOOP ( 'NONE', ( #8454, #12845, #4975, #817 ) ) ;
#13097 = VECTOR ( 'NONE', #10061, 1000.000000000000000 ) ;
#13098 = CARTESIAN_POINT ( 'NONE',  ( 1.493882881115753847, -0.7724999999999562217, -3.610279343491855641 ) ) ;
#13099 = DIRECTION ( 'NONE',  ( 1.000000000000000000, 0.000000000000000000, 0.000000000000000000 ) ) ;
#13100 = DIRECTION ( 'NONE',  ( 0.000000000000000000, 1.000000000000000000, 0.000000000000000000 ) ) ;
#13101 = DIRECTION ( 'NONE',  ( 0.000000000000000000, -1.000000000000000000, -0.000000000000000000 ) ) ;
#13102 = CARTESIAN_POINT ( 'NONE',  ( 22.58164641901421632, -12.50000029085423847, -8.775548064764199907 ) ) ;
#13103 = FACE_OUTER_BOUND ( 'NONE', #983, .T. ) ;
#13104 = CYLINDRICAL_SURFACE ( 'NONE', #6353, 4.499999999999997335 ) ;
#13105 = AXIS2_PLACEMENT_3D ( 'NONE', #10597, #4714, #13018 ) ;
#13106 = ORIENTED_EDGE ( 'NONE', *, *, #5470, .T. ) ;
#13107 = LINE ( 'NONE', #7365, #10230 ) ;
#13108 = CARTESIAN_POINT ( 'NONE',  ( 16.96309080958207360, 41.51006470759390510, 57.31273383969018198 ) ) ;
#13109 = EDGE_CURVE ( 'NONE', #858, #10812, #1801, .T. ) ;
#13110 = ORIENTED_EDGE ( 'NONE', *, *, #698, .T. ) ;
#13111 = DIRECTION ( 'NONE',  ( 0.000000000000000000, 0.000000000000000000, 1.000000000000000000 ) ) ;
#13112 = CARTESIAN_POINT ( 'NONE',  ( -0.7073002561900944007, -2.866249999999988418, -3.560643744722165938 ) ) ;
#13113 = ORIENTED_EDGE ( 'NONE', *, *, #7828, .F. ) ;
#13114 = ORIENTED_EDGE ( 'NONE', *, *, #2314, .F. ) ;
#13115 = ORIENTED_EDGE ( 'NONE', *, *, #9402, .T. ) ;
#13116 = DIRECTION ( 'NONE',  ( 0.000000000000000000, 0.000000000000000000, 1.000000000000000000 ) ) ;
#13117 = DIRECTION ( 'NONE',  ( -1.000000000000000000, 0.000000000000000000, 0.000000000000000000 ) ) ;
#13118 = CARTESIAN_POINT ( 'NONE',  ( -51.75338362643999801, 63.40569462133917256, -147.9984795835769944 ) ) ;
#13119 = CARTESIAN_POINT ( 'NONE',  ( 21.98164641901421135, -12.60000029085423812, -8.183940086454239093 ) ) ;
#13120 = CARTESIAN_POINT ( 'NONE',  ( -50.73238362643999722, 63.99516924618178848, -150.4984795835770228 ) ) ;
#13121 = FACE_BOUND ( 'NONE', #8532, .T. ) ;
#13122 = EDGE_CURVE ( 'NONE', #6604, #6326, #5795, .T. ) ;
#13123 = CARTESIAN_POINT ( 'NONE',  ( -2.211816241884709822, -3.944375000000018172, -2.696513105594267046 ) ) ;
#13124 = DIRECTION ( 'NONE',  ( -1.000000000000000000, 0.000000000000000000, 0.000000000000000000 ) ) ;
#13125 = VERTEX_POINT ( 'NONE', #8295 ) ;
#13126 = DIRECTION ( 'NONE',  ( -0.000000000000000000, -0.000000000000000000, 1.000000000000000000 ) ) ;
#13127 = ORIENTED_EDGE ( 'NONE', *, *, #12344, .F. ) ;
#13128 = ORIENTED_EDGE ( 'NONE', *, *, #13702, .T. ) ;
#13129 = VERTEX_POINT ( 'NONE', #1519 ) ;
#13130 =( LENGTH_UNIT ( ) NAMED_UNIT ( * ) SI_UNIT ( .MILLI., .METRE. ) );
#13131 = CARTESIAN_POINT ( 'NONE',  ( 0.3508518002069317410, -3.350624999999907150, 3.548798009676430887 ) ) ;
#13132 = B_SPLINE_CURVE_WITH_KNOTS ( 'NONE', 3,
 ( #2268, #3747, #4761, #9477, #14217, #8407 ),
 .UNSPECIFIED., .F., .F.,
 ( 4, 2, 4 ),
 ( 1.820537833122031213, 2.555393473688635453, 3.290249114255239693 ),
 .UNSPECIFIED. ) ;
#13133 = CARTESIAN_POINT ( 'NONE',  ( 14.66434062215688883, -0.3156604612129069731, 21.53909249377453250 ) ) ;
#13134 = CARTESIAN_POINT ( 'NONE',  ( 22.58164641901420921, -3.623250966006795970, 0.01788390626213397228 ) ) ;
#13135 = DIRECTION ( 'NONE',  ( 0.000000000000000000, 1.000000000000000000, 0.000000000000000000 ) ) ;
#13136 = LINE ( 'NONE', #7236, #1152 ) ;
#13137 = DIRECTION ( 'NONE',  ( 1.000000000000000000, 9.422394424380278809E-16, 0.000000000000000000 ) ) ;
#13138 = CARTESIAN_POINT ( 'NONE',  ( -72.41519636940742544, 89.17411849586704875, -44.45439862457369884 ) ) ;
#13139 = DIRECTION ( 'NONE',  ( 0.000000000000000000, -4.336808689942017736E-16, 1.000000000000000000 ) ) ;
#13140 = EDGE_CURVE ( 'NONE', #7562, #11318, #7278, .T. ) ;
#13141 = CARTESIAN_POINT ( 'NONE',  ( 16.58164641901421277, 11.39999970914575833, 0.2664120436859911956 ) ) ;
#13142 = DIRECTION ( 'NONE',  ( 0.000000000000000000, 0.000000000000000000, -1.000000000000000000 ) ) ;
#13143 = ORIENTED_EDGE ( 'NONE', *, *, #4941, .F. ) ;
#13144 = CARTESIAN_POINT ( 'NONE',  ( 16.95292505576233566, -11.57157634197346852, 0.2884589904497822932 ) ) ;
#13145 = ORIENTED_EDGE ( 'NONE', *, *, #11226, .T. ) ;
#13146 = ADVANCED_FACE ( 'NONE', ( #6275 ), #5486, .F. ) ;
#13147 = EDGE_LOOP ( 'NONE', ( #15152, #1462, #499, #4190, #4949 ) ) ;
#13148 = VERTEX_POINT ( 'NONE', #2995 ) ;
#13149 = CARTESIAN_POINT ( 'NONE',  ( 15.14695642955105193, -1.094824204497501265E-15, 22.92302504315390621 ) ) ;
#13150 = ORIENTED_EDGE ( 'NONE', *, *, #4762, .T. ) ;
#13151 = CARTESIAN_POINT ( 'NONE',  ( 2.995266967284331283, -1.124213562373126862, -2.993673064536260142 ) ) ;
#13152 = EDGE_CURVE ( 'NONE', #9494, #5961, #11598, .T. ) ;
#13153 = CARTESIAN_POINT ( 'NONE',  ( -104.2743836264399988, 60.67411849586700612, -67.49847958357700861 ) ) ;
#13154 = FACE_BOUND ( 'NONE', #10052, .T. ) ;
#13155 = DIRECTION ( 'NONE',  ( 0.000000000000000000, 0.000000000000000000, -1.000000000000000000 ) ) ;
#13156 = EDGE_CURVE ( 'NONE', #4417, #4564, #13773, .T. ) ;
#13157 = FACE_OUTER_BOUND ( 'NONE', #8437, .T. ) ;
#13158 = EDGE_LOOP ( 'NONE', ( #350, #6909, #652, #7015 ) ) ;
#13159 = CYLINDRICAL_SURFACE ( 'NONE', #13315, 4.000000000000000000 ) ;
#13160 = B_SPLINE_CURVE_WITH_KNOTS ( 'NONE', 3,
 ( #5547, #5468, #14978, #10166, #1888, #4371, #10101, #14834, #7934, #4218, #11354, #5315, #10029, #3052, #3131, #11502, #9094, #8942, #12524, #4446, #720, #564, #2036, #6643, #867, #9165, #13904, #14900, #8004, #1732 ),
 .UNSPECIFIED., .F., .F.,
 ( 4, 2, 2, 2, 2, 2, 2, 2, 2, 2, 2, 2, 2, 2, 4 ),
 ( 0.000000000000000000, 0.0006682858881741897015, 0.001336571776348379403, 0.002004857664522568996, 0.002673143552696758806, 0.003341429440870947749, 0.004009715329045136258, 0.004678001217219326067, 0.005346287105393515010, 0.006014572993567703953, 0.006682858881741892028, 0.007351144769916080970, 0.008019430658090269046, 0.009356002434438646931, 0.01069257421078702308 ),
 .UNSPECIFIED. ) ;
#13161 = CARTESIAN_POINT ( 'NONE',  ( -35.58670980944424400, 2.488961461112888074, 131.2954986191910791 ) ) ;
#13162 = SHAPE_DEFINITION_REPRESENTATION ( #503, #5010 ) ;
#13163 = VERTEX_POINT ( 'NONE', #13921 ) ;
#13164 = CARTESIAN_POINT ( 'NONE',  ( -2.667345689317278890, -4.625000000000156319, 2.665957393838279010 ) ) ;
#13165 = VERTEX_POINT ( 'NONE', #9178 ) ;
#13166 = CARTESIAN_POINT ( 'NONE',  ( -3.224082633657694430, -0.9912500000000042943, -2.155484159616896989 ) ) ;
#13167 = DIRECTION ( 'NONE',  ( 1.000000000000000000, 0.000000000000000000, 0.000000000000000000 ) ) ;
#13168 = LINE ( 'NONE', #4944, #1601 ) ;
#13169 = AXIS2_PLACEMENT_3D ( 'NONE', #1445, #6201, #10665 ) ;
#13170 = CARTESIAN_POINT ( 'NONE',  ( 0.000000000000000000, 0.000000000000000000, 0.000000000000000000 ) ) ;
#13171 = CARTESIAN_POINT ( 'NONE',  ( 3.406229051843177036, -5.265617073852581598, 0.7216417731445288197 ) ) ;
#13172 = DIRECTION ( 'NONE',  ( -1.000000000000000000, 0.000000000000000000, 0.000000000000000000 ) ) ;
#13173 = LINE ( 'NONE', #7284, #13551 ) ;
#13174 = CIRCLE ( 'NONE', #12678, 2.042000000000002036 ) ;
#13175 = ORIENTED_EDGE ( 'NONE', *, *, #8478, .F. ) ;
#13176 = FACE_OUTER_BOUND ( 'NONE', #11283, .T. ) ;
#13177 = ORIENTED_EDGE ( 'NONE', *, *, #8878, .F. ) ;
#13178 = CYLINDRICAL_SURFACE ( 'NONE', #12503, 1.250000000000001110 ) ;
#13179 = CARTESIAN_POINT ( 'NONE',  ( 1.974738715674900114, -3.428749999999933795, 2.957050713271640152 ) ) ;
#13180 = ORIENTED_EDGE ( 'NONE', *, *, #14622, .F. ) ;
#13181 = ORIENTED_EDGE ( 'NONE', *, *, #5767, .F. ) ;
#13182 = ORIENTED_EDGE ( 'NONE', *, *, #14163, .F. ) ;
#13183 = AXIS2_PLACEMENT_3D ( 'NONE', #7185, #98, #7254 ) ;
#13184 = DIRECTION ( 'NONE',  ( 0.000000000000000000, 1.000000000000000000, 0.000000000000000000 ) ) ;
#13185 = AXIS2_PLACEMENT_3D ( 'NONE', #3727, #6002, #11953 ) ;
#13186 = CARTESIAN_POINT ( 'NONE',  ( -2.802265715718426975, 1.883037081658663903, 4.146333404067328310 ) ) ;
#13187 = AXIS2_PLACEMENT_3D ( 'NONE', #1911, #13634, #10120 ) ;
#13188 = EDGE_CURVE ( 'NONE', #7307, #7295, #6802, .T. ) ;
#13189 = LINE ( 'NONE', #4893, #4816 ) ;
#13190 = DIRECTION ( 'NONE',  ( -1.284980352575412699E-16, 0.000000000000000000, -1.000000000000000000 ) ) ;
#13191 = DIRECTION ( 'NONE',  ( 0.000000000000000000, 0.000000000000000000, -1.000000000000000000 ) ) ;
#13192 = CARTESIAN_POINT ( 'NONE',  ( 3.389189273868536745, -3.538124999999807674, 1.026728768593236030 ) ) ;
#13193 = CARTESIAN_POINT ( 'NONE',  ( -15.50000000000000000, 0.000000000000000000, -22.50000000000000000 ) ) ;
#13194 = VECTOR ( 'NONE', #12738, 1000.000000000000000 ) ;
#13195 = VERTEX_POINT ( 'NONE', #3293 ) ;
#13196 = DIRECTION ( 'NONE',  ( 0.000000000000000000, 0.000000000000000000, -1.000000000000000000 ) ) ;
#13197 = ORIENTED_EDGE ( 'NONE', *, *, #8308, .F. ) ;
#13198 = ORIENTED_EDGE ( 'NONE', *, *, #1070, .T. ) ;
#13199 = ORIENTED_EDGE ( 'NONE', *, *, #5559, .F. ) ;
#13200 = ORIENTED_EDGE ( 'NONE', *, *, #7668, .F. ) ;
#13201 = CIRCLE ( 'NONE', #302, 0.9999999999999957812 ) ;
#13202 = EDGE_CURVE ( 'NONE', #7541, #10234, #734, .T. ) ;
#13203 = CARTESIAN_POINT ( 'NONE',  ( 0.3421672931281763419, -3.819374999999898268, -3.487344533451358863 ) ) ;
#13204 = CARTESIAN_POINT ( 'NONE',  ( -6.060835862730317059E-15, 2.375000000000000000, 0.000000000000000000 ) ) ;
#13205 = CARTESIAN_POINT ( 'NONE',  ( -0.3668491701747607636, -4.734375000000160760, 3.738752075031570588 ) ) ;
#13206 = FACE_BOUND ( 'NONE', #4889, .T. ) ;
#13207 = ADVANCED_FACE ( 'NONE', ( #808 ), #5298, .T. ) ;
#13208 = CARTESIAN_POINT ( 'NONE',  ( 15.50000000000000000, -0.2038245569916610489, 21.05662432702600029 ) ) ;
#13209 = LINE ( 'NONE', #1328, #4398 ) ;
#13210 = CARTESIAN_POINT ( 'NONE',  ( -65.73898050152220662, 64.78624853950366003, -81.84847958357697451 ) ) ;
#13211 = FACE_OUTER_BOUND ( 'NONE', #554, .T. ) ;
#13212 = VECTOR ( 'NONE', #11172, 1000.000000000000000 ) ;
#13213 = DIRECTION ( 'NONE',  ( 0.000000000000000000, 0.000000000000000000, 1.000000000000000000 ) ) ;
#13214 = DIRECTION ( 'NONE',  ( 0.000000000000000000, 0.000000000000000000, 1.000000000000000000 ) ) ;
#13215 = ORIENTED_EDGE ( 'NONE', *, *, #12019, .T. ) ;
#13216 = CARTESIAN_POINT ( 'NONE',  ( -23.24999999999999289, 0.000000000000000000, 27.00000000000000000 ) ) ;
#13217 = VERTEX_POINT ( 'NONE', #3148 ) ;
#13218 = TOROIDAL_SURFACE ( 'NONE', #6535, 2.700000000000000178, 0.2000000000000000111 ) ;
#13219 = ORIENTED_EDGE ( 'NONE', *, *, #2584, .T. ) ;
#13220 = LINE ( 'NONE', #9329, #8955 ) ;
#13221 = CARTESIAN_POINT ( 'NONE',  ( -53.77438362644000591, 82.17411849586700612, -117.9984795835769944 ) ) ;
#13222 = EDGE_CURVE ( 'NONE', #6563, #8835, #1579, .T. ) ;
#13223 = CARTESIAN_POINT ( 'NONE',  ( -2.388143517671037941, -0.6554635623729724303, 3.572045695433365697 ) ) ;
#13224 = CIRCLE ( 'NONE', #3297, 1.500000000000001332 ) ;
#13225 = DIRECTION ( 'NONE',  ( 0.000000000000000000, 1.000000000000000000, 0.000000000000000000 ) ) ;
#13226 = CYLINDRICAL_SURFACE ( 'NONE', #6496, 16.50000000000000000 ) ;
#13227 = EDGE_CURVE ( 'NONE', #12491, #7325, #8261, .T. ) ;
#13228 = DIRECTION ( 'NONE',  ( 0.000000000000000000, 1.000000000000000000, 0.000000000000000000 ) ) ;
#13229 = VECTOR ( 'NONE', #464, 1000.000000000000000 ) ;
#13230 = CARTESIAN_POINT ( 'NONE',  ( -35.58670980944424400, 5.000000000000000000, 95.72362361919107343 ) ) ;
#13231 = DIRECTION ( 'NONE',  ( 1.000000000000000000, 0.000000000000000000, 0.000000000000000000 ) ) ;
#13232 = VERTEX_POINT ( 'NONE', #1976 ) ;
#13233 = CARTESIAN_POINT ( 'NONE',  ( -55.52438362644000591, 65.17411849586700612, -86.49847958357699440 ) ) ;
#13234 = CIRCLE ( 'NONE', #9750, 3.968749999999992895 ) ;
#13235 = AXIS2_PLACEMENT_3D ( 'NONE', #4028, #7686, #535 ) ;
#13236 = ADVANCED_FACE ( 'NONE', ( #7730 ), #14203, .F. ) ;
#13237 = EDGE_CURVE ( 'NONE', #1968, #12943, #15073, .T. ) ;
#13238 = VERTEX_POINT ( 'NONE', #9110 ) ;
#13239 = CARTESIAN_POINT ( 'NONE',  ( 17.12895037488186389, 3.654026927208769315, 0.2687305842673423095 ) ) ;
#13240 = CARTESIAN_POINT ( 'NONE',  ( 1.432789758436758154, -4.812499999999716671, 3.461605376534508505 ) ) ;
#13241 = ORIENTED_EDGE ( 'NONE', *, *, #3186, .T. ) ;
#13242 = ADVANCED_FACE ( 'NONE', ( #14777 ), #7808, .T. ) ;
#13243 = CARTESIAN_POINT ( 'NONE',  ( 3.730555813499059070, -1.553749999999926246, 0.7430650243616524486 ) ) ;
#13244 = CIRCLE ( 'NONE', #7564, 8.000000000000007105 ) ;
#13245 = AXIS2_PLACEMENT_3D ( 'NONE', #9193, #4788, #5730 ) ;
#13246 = EDGE_CURVE ( 'NONE', #11128, #12756, #7095, .T. ) ;
#13247 = CARTESIAN_POINT ( 'NONE',  ( 0.1494771202956585165, -5.386673054885917189, 3.320955697048893818 ) ) ;
#13248 = EDGE_CURVE ( 'NONE', #14841, #1774, #11292, .T. ) ;
#13249 = CARTESIAN_POINT ( 'NONE',  ( 0.06617338034656250478, 5.102742169785384244E-16, 17.58834813908115180 ) ) ;
#13250 = DIRECTION ( 'NONE',  ( 0.000000000000000000, 0.000000000000000000, 1.000000000000000000 ) ) ;
#13251 = CARTESIAN_POINT ( 'NONE',  ( 3.267958496119054423, -5.289367998540840610, 1.137001996541352034 ) ) ;
#13252 = DIRECTION ( 'NONE',  ( -1.000000000000000000, 0.000000000000000000, 0.000000000000000000 ) ) ;
#13253 = PLANE ( 'NONE',  #2373 ) ;
#13254 = EDGE_LOOP ( 'NONE', ( #8755, #3512, #10444, #8804, #917, #4760 ) ) ;
#13255 = DIRECTION ( 'NONE',  ( 0.000000000000000000, 0.000000000000000000, -1.000000000000000000 ) ) ;
#13256 = CLOSED_SHELL ( 'NONE', ( #2466, #1956, #7184, #14840, #4958, #8578, #296, #13353, #8637, #6705, #2973, #12560, #13789, #6574, #9317, #11620, #6033, #1471, #9009, #9419, #9607, #11780, #5619, #4703, #9246, #13503, #9159, #8257, #4983, #431, #4425, #4410, #39, #5080, #4674, #12183, #4303, #1805, #2042, #9189, #3853, #13974, #12004, #3677, #15303, #3440, #12595, #8679, #2594, #15308, #12098, #14037, #1004, #10517, #13242, #3146, #4786 ) ) ;
#13257 = DIRECTION ( 'NONE',  ( 1.000000000000000000, 0.000000000000000000, 0.000000000000000000 ) ) ;
#13258 = AXIS2_PLACEMENT_3D ( 'NONE', #12666, #10401, #10331 ) ;
#13259 = EDGE_LOOP ( 'NONE', ( #7662, #4839, #12341, #12706 ) ) ;
#13260 = CARTESIAN_POINT ( 'NONE',  ( 22.58164641901421632, 11.99999970914576686, -14.73358795631400575 ) ) ;
#13261 = VERTEX_POINT ( 'NONE', #4165 ) ;
#13262 = ORIENTED_EDGE ( 'NONE', *, *, #13386, .T. ) ;
#13263 = VERTEX_POINT ( 'NONE', #6577 ) ;
#13264 = CARTESIAN_POINT ( 'NONE',  ( -77.94906324475290660, 70.01464610989972925, -81.84847958357697451 ) ) ;
#13265 = CARTESIAN_POINT ( 'NONE',  ( -3.265322824347066444, -5.249359343367779651, -1.273401769415555496 ) ) ;
#13266 = CARTESIAN_POINT ( 'NONE',  ( -4.522482571421200248, -85.69524470659703752, 70.03692566716173928 ) ) ;
#13267 = AXIS2_PLACEMENT_3D ( 'NONE', #10712, #9235, #1013 ) ;
#13268 = DIRECTION ( 'NONE',  ( 0.000000000000000000, 0.000000000000000000, -1.000000000000000000 ) ) ;
#13269 = SURFACE_STYLE_FILL_AREA ( #1309 ) ;
#13270 = AXIS2_PLACEMENT_3D ( 'NONE', #13520, #2803, #8545 ) ;
#13271 = FACE_OUTER_BOUND ( 'NONE', #11694, .T. ) ;
#13272 = B_SPLINE_CURVE_WITH_KNOTS ( 'NONE', 3,
 ( #1802, #15055, #641, #13681 ),
 .UNSPECIFIED., .F., .F.,
 ( 4, 4 ),
 ( 0.002598307151460989804, 0.005196383362814306975 ),
 .UNSPECIFIED. ) ;
#13273 = CARTESIAN_POINT ( 'NONE',  ( -1.038475776471825762, -3.288125000000012843, 3.420226703972062854 ) ) ;
#13274 = CARTESIAN_POINT ( 'NONE',  ( -2.598076211353316012, 0.1227504548087343245, -4.499999999999999112 ) ) ;
#13275 = ORIENTED_EDGE ( 'NONE', *, *, #5474, .F. ) ;
#13276 = DIRECTION ( 'NONE',  ( 0.000000000000000000, 0.000000000000000000, -1.000000000000000000 ) ) ;
#13277 = ORIENTED_EDGE ( 'NONE', *, *, #12447, .T. ) ;
#13278 = ORIENTED_EDGE ( 'NONE', *, *, #10279, .F. ) ;
#13279 = ORIENTED_EDGE ( 'NONE', *, *, #12297, .F. ) ;
#13280 = AXIS2_PLACEMENT_3D ( 'NONE', #10354, #971, #5723 ) ;
#13281 = ORIENTED_EDGE ( 'NONE', *, *, #1359, .F. ) ;
#13282 = VECTOR ( 'NONE', #7843, 1000.000000000000000 ) ;
#13283 = FACE_OUTER_BOUND ( 'NONE', #7062, .T. ) ;
#13284 = AXIS2_PLACEMENT_3D ( 'NONE', #10863, #5127, #14571 ) ;
#13285 = CARTESIAN_POINT ( 'NONE',  ( 3.109021928378527200, -3.663124999999927578, -1.660781358202984448 ) ) ;
#13286 = CARTESIAN_POINT ( 'NONE',  ( 3.701456747302541928, -5.015624999999988454, -0.3659357139933352987 ) ) ;
#13287 = CARTESIAN_POINT ( 'NONE',  ( -90.85838362644101096, 99.17411849586700612, -147.9984795835769944 ) ) ;
#13288 = DIRECTION ( 'NONE',  ( -1.000000000000000000, -2.551930889570659960E-15, 0.000000000000000000 ) ) ;
#13289 = CARTESIAN_POINT ( 'NONE',  ( -88.81638362644100937, 97.99516924618178848, -150.4984795835770228 ) ) ;
#13290 = CARTESIAN_POINT ( 'NONE',  ( 16.18545172092247242, 11.99999970914575798, -0.4207436990616704175 ) ) ;
#13291 = CIRCLE ( 'NONE', #14990, 3.173335668876520188 ) ;
#13292 = CARTESIAN_POINT ( 'NONE',  ( -35.58670980944424400, 0.000000000000000000, 129.5095611191910621 ) ) ;
#13293 = DIRECTION ( 'NONE',  ( -1.000000000000000000, -2.551930889570659565E-15, 0.000000000000000000 ) ) ;
#13294 = CARTESIAN_POINT ( 'NONE',  ( -52.77438362644100067, 99.17411849586700612, -145.2984795835770058 ) ) ;
#13295 = TOROIDAL_SURFACE ( 'NONE', #7595, 3.299999999999470024, 0.2000000000005275058 ) ;
#13296 = EDGE_LOOP ( 'NONE', ( #1063, #1023, #5694, #9884 ) ) ;
#13297 = CIRCLE ( 'NONE', #645, 2.750000000000002665 ) ;
#13298 = CARTESIAN_POINT ( 'NONE',  ( -57.27438362643999881, 65.17411849586700612, -79.59847958357700293 ) ) ;
#13299 = EDGE_CURVE ( 'NONE', #14910, #6904, #659, .T. ) ;
#13300 = ORIENTED_EDGE ( 'NONE', *, *, #13613, .F. ) ;
#13301 = ORIENTED_EDGE ( 'NONE', *, *, #11812, .T. ) ;
#13302 = CARTESIAN_POINT ( 'NONE',  ( -1.520556115814812870, -5.913125000000218456, -2.846480943363819627 ) ) ;
#13303 = EDGE_CURVE ( 'NONE', #9206, #15023, #11889, .T. ) ;
#13304 = CARTESIAN_POINT ( 'NONE',  ( 3.856928834949548079, -0.07812500000007562007, -2.060244425025098192 ) ) ;
#13305 = AXIS2_PLACEMENT_3D ( 'NONE', #8508, #3933, #10913 ) ;
#13306 = CARTESIAN_POINT ( 'NONE',  ( -3.858379451542089278, -1.561713562373104214, 1.599828451265935536 ) ) ;
#13307 = VECTOR ( 'NONE', #9542, 999.9999999999998863 ) ;
#13308 = PLANE ( 'NONE',  #5877 ) ;
#13309 = AXIS2_PLACEMENT_3D ( 'NONE', #14582, #1411, #9769 ) ;
#13310 = DIRECTION ( 'NONE',  ( 0.000000000000000000, 1.000000000000000000, 0.000000000000000000 ) ) ;
#13311 = FACE_OUTER_BOUND ( 'NONE', #2441, .T. ) ;
#13312 = CARTESIAN_POINT ( 'NONE',  ( -52.77438362643999881, 65.17411849586700612, -182.2484795835770228 ) ) ;
#13313 = CYLINDRICAL_SURFACE ( 'NONE', #9424, 3.000000000000000888 ) ;
#13314 = ORIENTED_EDGE ( 'NONE', *, *, #15221, .T. ) ;
#13315 = AXIS2_PLACEMENT_3D ( 'NONE', #9645, #1439, #3842 ) ;
#13316 = DIRECTION ( 'NONE',  ( -0.000000000000000000, 1.000000000000000000, -0.000000000000000000 ) ) ;
#13317 = EDGE_CURVE ( 'NONE', #8152, #8702, #1065, .T. ) ;
#13318 = AXIS2_PLACEMENT_3D ( 'NONE', #10007, #10147, #7847 ) ;
#13319 = ORIENTED_EDGE ( 'NONE', *, *, #11573, .F. ) ;
#13320 = CARTESIAN_POINT ( 'NONE',  ( -3.138285373062238648, -4.593749999999839240, 2.098600886432549828 ) ) ;
#13321 = ORIENTED_EDGE ( 'NONE', *, *, #6742, .F. ) ;
#13322 = CARTESIAN_POINT ( 'NONE',  ( 1.089607726473704297, -4.796088562373097552, 3.587212734375584411 ) ) ;
#13323 = VECTOR ( 'NONE', #8799, 1000.000000000000000 ) ;
#13324 = CARTESIAN_POINT ( 'NONE',  ( 1.801006600569655891, -1.413124999999811449, 3.371562913404185569 ) ) ;
#13325 = CARTESIAN_POINT ( 'NONE',  ( -2.598076211353319120, 1.678847577293364424, 4.500000000000000888 ) ) ;
#13326 = AXIS2_PLACEMENT_3D ( 'NONE', #4712, #337, #4638 ) ;
#13327 = EDGE_CURVE ( 'NONE', #3176, #2123, #2555, .T. ) ;
#13328 = DIRECTION ( 'NONE',  ( -0.9375000000000006661, 0.000000000000000000, -0.3479852726768744020 ) ) ;
#13329 = CARTESIAN_POINT ( 'NONE',  ( -86.77438362644100778, 99.17411849586700612, -79.59847958357700293 ) ) ;
#13330 = LINE ( 'NONE', #6277, #10353 ) ;
#13331 = CARTESIAN_POINT ( 'NONE',  ( -2.320576762250993852, 9.355654565435171932, 3.410994500647662804E-16 ) ) ;
#13332 = CARTESIAN_POINT ( 'NONE',  ( -35.58670980944424400, 5.000000000000000000, 97.50956111919106206 ) ) ;
#13333 = DIRECTION ( 'NONE',  ( 0.9999934663667179313, -1.567696289299852222E-18, 0.003614861529252313445 ) ) ;
#13334 = EDGE_CURVE ( 'NONE', #9205, #2361, #11472, .T. ) ;
#13335 = ORIENTED_EDGE ( 'NONE', *, *, #10492, .T. ) ;
#13336 = ORIENTED_EDGE ( 'NONE', *, *, #6717, .T. ) ;
#13337 = ORIENTED_EDGE ( 'NONE', *, *, #14835, .F. ) ;
#13338 = EDGE_CURVE ( 'NONE', #9368, #4210, #11905, .T. ) ;
#13339 = VECTOR ( 'NONE', #8776, 1000.000000000000114 ) ;
#13340 = DIRECTION ( 'NONE',  ( -1.000000000000000000, -0.000000000000000000, -0.000000000000000000 ) ) ;
#13341 = EDGE_CURVE ( 'NONE', #5823, #13360, #13086, .T. ) ;
#13342 = CARTESIAN_POINT ( 'NONE',  ( 3.244093391032127016, -2.506875000000020837, 1.732468392772113841 ) ) ;
#13343 = ORIENTED_EDGE ( 'NONE', *, *, #13714, .T. ) ;
#13344 = ORIENTED_EDGE ( 'NONE', *, *, #14370, .F. ) ;
#13345 = LINE ( 'NONE', #2629, #6482 ) ;
#13346 = ADVANCED_FACE ( 'NONE', ( #9340 ), #1198, .T. ) ;
#13347 = CARTESIAN_POINT ( 'NONE',  ( 0.7350389054958545998, -5.152513402290675337, -3.570507098978675131 ) ) ;
#13348 = LINE ( 'NONE', #2777, #9025 ) ;
#13349 = AXIS2_PLACEMENT_3D ( 'NONE', #9774, #6395, #14508 ) ;
#13350 = DIRECTION ( 'NONE',  ( 1.000000000000000000, 0.000000000000000000, 0.000000000000000000 ) ) ;
#13351 = CARTESIAN_POINT ( 'NONE',  ( 10.10406781373725771, -85.69524470659703752, 69.08979243323349806 ) ) ;
#13352 = CARTESIAN_POINT ( 'NONE',  ( -61.42438362644001160, 82.17411849586700612, -80.14847958357698587 ) ) ;
#13353 = ADVANCED_FACE ( 'NONE', ( #1119 ), #3447, .T. ) ;
#13354 = LINE ( 'NONE', #2711, #9984 ) ;
#13355 = ORIENTED_EDGE ( 'NONE', *, *, #713, .T. ) ;
#13356 = CARTESIAN_POINT ( 'NONE',  ( -52.77438362643999881, 65.17411849586700612, -182.2484795835770228 ) ) ;
#13357 = ORIENTED_EDGE ( 'NONE', *, *, #2908, .F. ) ;
#13358 = ORIENTED_EDGE ( 'NONE', *, *, #8726, .T. ) ;
#13359 = VERTEX_POINT ( 'NONE', #15145 ) ;
#13360 = VERTEX_POINT ( 'NONE', #2508 ) ;
#13361 = CIRCLE ( 'NONE', #10112, 2.750000000000002665 ) ;
#13362 = FACE_OUTER_BOUND ( 'NONE', #3016, .T. ) ;
#13363 = CARTESIAN_POINT ( 'NONE',  ( -3.093239089446854884, -2.178749999999916476, 2.068481483294962953 ) ) ;
#13364 = CARTESIAN_POINT ( 'NONE',  ( 0.3862366009532263167, -3.234374999999897859, -3.936230821419137271 ) ) ;
#13365 = DIRECTION ( 'NONE',  ( 0.3469356515732584523, -0.9378889346118967074, 0.000000000000000000 ) ) ;
#13366 = CARTESIAN_POINT ( 'NONE',  ( -101.2743836264399988, 114.1741184958669777, -79.49847958357700861 ) ) ;
#13367 = CARTESIAN_POINT ( 'NONE',  ( -86.77438362644001302, 99.17411849586700612, -86.49847958357699440 ) ) ;
#13368 = DIRECTION ( 'NONE',  ( -1.000000000000000000, 0.000000000000000000, 0.000000000000000000 ) ) ;
#13369 = DIRECTION ( 'NONE',  ( 0.8660254037844383745, -0.5000000000000003331, 0.000000000000000000 ) ) ;
#13370 = CARTESIAN_POINT ( 'NONE',  ( -15.50000000000000000, -0.2038245569916614930, -21.05662432702600029 ) ) ;
#13371 = DIRECTION ( 'NONE',  ( -0.8660254037844387076, -0.4999999999999998890, 0.000000000000000000 ) ) ;
#13372 = ORIENTED_EDGE ( 'NONE', *, *, #4620, .T. ) ;
#13373 = DIRECTION ( 'NONE',  ( 0.000000000000000000, -0.000000000000000000, -1.000000000000000000 ) ) ;
#13374 = ORIENTED_EDGE ( 'NONE', *, *, #14092, .F. ) ;
#13375 = VERTEX_POINT ( 'NONE', #10581 ) ;
#13376 = ORIENTED_EDGE ( 'NONE', *, *, #6903, .F. ) ;
#13377 = UNCERTAINTY_MEASURE_WITH_UNIT (LENGTH_MEASURE( 1.000000000000000082E-05 ), #11146, 'distance_accuracy_value', 'NONE');
#13378 = CARTESIAN_POINT ( 'NONE',  ( -0.3227798623957894852, -5.319375000000161613, 3.289865787063878777 ) ) ;
#13379 = DIRECTION ( 'NONE',  ( 0.000000000000000000, 0.000000000000000000, 1.000000000000000000 ) ) ;
#13380 = CARTESIAN_POINT ( 'NONE',  ( -3.199287326323787095, -5.038124999999881837, -0.9691876696830878934 ) ) ;
#13381 = CARTESIAN_POINT ( 'NONE',  ( -86.77438362644001302, 99.17411849586700612, -145.4984795835769660 ) ) ;
#13382 = CARTESIAN_POINT ( 'NONE',  ( -89.52438362644001302, 65.17411849586700612, -152.4984795835769944 ) ) ;
#13383 = CARTESIAN_POINT ( 'NONE',  ( -80.27438362643999881, 82.17411849586700612, -80.44847958357698303 ) ) ;
#13384 = FACE_OUTER_BOUND ( 'NONE', #6199, .T. ) ;
#13385 = PLANE ( 'NONE',  #1822 ) ;
#13386 = EDGE_CURVE ( 'NONE', #6471, #14595, #2048, .T. ) ;
#13387 = PLANE ( 'NONE',  #10671 ) ;
#13388 = EDGE_LOOP ( 'NONE', ( #11205, #11891 ) ) ;
#13389 = LINE ( 'NONE', #9722, #7115 ) ;
#13390 = ORIENTED_EDGE ( 'NONE', *, *, #514, .T. ) ;
#13391 = CARTESIAN_POINT ( 'NONE',  ( 0.4017167453136591404, -2.234374999999921396, -4.067671435978028605 ) ) ;
#13392 = ORIENTED_EDGE ( 'NONE', *, *, #9297, .F. ) ;
#13393 = CARTESIAN_POINT ( 'NONE',  ( -3.159664717618257956, -4.405463562373036268, -2.112412258076255878 ) ) ;
#13394 = DIRECTION ( 'NONE',  ( 0.000000000000000000, 0.000000000000000000, -1.000000000000000000 ) ) ;
#13395 = ADVANCED_FACE ( 'NONE', ( #8344 ), #7187, .F. ) ;
#13396 = CARTESIAN_POINT ( 'NONE',  ( -12.81835358098578759, -12.00000029085424202, -0.3335879563140091153 ) ) ;
#13397 = DIRECTION ( 'NONE',  ( -3.614007241618342978E-17, -1.000000000000000000, -0.000000000000000000 ) ) ;
#13398 = DIRECTION ( 'NONE',  ( 0.9961946980917453232, -7.200509705930740925E-17, 0.08715574274766159368 ) ) ;
#13399 = ADVANCED_FACE ( 'NONE', ( #3521 ), #8106, .F. ) ;
#13400 = CARTESIAN_POINT ( 'NONE',  ( -86.77438362643999881, 65.17411849586700612, -147.9984795835769944 ) ) ;
#13401 = DIRECTION ( 'NONE',  ( 0.000000000000000000, 1.000000000000000000, 0.000000000000000000 ) ) ;
#13402 = DIRECTION ( 'NONE',  ( 0.000000000000000000, 0.000000000000000000, -1.000000000000000000 ) ) ;
#13403 = DIRECTION ( 'NONE',  ( -0.8660254037844482555, 0.000000000000000000, 0.4999999999999831801 ) ) ;
#13404 = CARTESIAN_POINT ( 'NONE',  ( 17.18164641901421419, 3.654316742536407592, 0.2664120436859910845 ) ) ;
#13405 = ORIENTED_EDGE ( 'NONE', *, *, #13677, .T. ) ;
#13406 = EDGE_LOOP ( 'NONE', ( #10529, #6606, #13452, #9438, #1142 ) ) ;
#13407 = EDGE_LOOP ( 'NONE', ( #13182, #3383 ) ) ;
#13408 = CARTESIAN_POINT ( 'NONE',  ( -2.931404194366994176, 4.650702586819535966, 0.000000000000000000 ) ) ;
#13409 = CARTESIAN_POINT ( 'NONE',  ( 0.001402937982463629916, -1.335000000000034825, 3.832736870811305874 ) ) ;
#13410 = ORIENTED_EDGE ( 'NONE', *, *, #1261, .F. ) ;
#13411 = EDGE_LOOP ( 'NONE', ( #13405, #12415 ) ) ;
#13412 = CARTESIAN_POINT ( 'NONE',  ( -69.77438362644001302, 82.17411849586700612, -79.49847958357700861 ) ) ;
#13413 = EDGE_CURVE ( 'NONE', #11838, #1588, #10738, .T. ) ;
#13414 = CARTESIAN_POINT ( 'NONE',  ( 15.50000000000000000, -0.4000000000000000222, 19.00000000000000355 ) ) ;
#13415 = LINE ( 'NONE', #11087, #3830 ) ;
#13416 = EDGE_CURVE ( 'NONE', #3042, #11390, #1812, .T. ) ;
#13417 = AXIS2_PLACEMENT_3D ( 'NONE', #1763, #14631, #2937 ) ;
#13418 = CARTESIAN_POINT ( 'NONE',  ( 2.348303809467377601, -0.4995676945082530018, -3.345954089472160664 ) ) ;
#13419 = CARTESIAN_POINT ( 'NONE',  ( 15.50000000000000000, -0.2038245569916604938, -21.05662432702600029 ) ) ;
#13420 = DIRECTION ( 'NONE',  ( 0.000000000000000000, 1.000000000000000000, 0.000000000000000000 ) ) ;
#13421 = CARTESIAN_POINT ( 'NONE',  ( -57.02438362644099357, 99.17411849586700612, -145.4984795835769660 ) ) ;
#13422 = ORIENTED_EDGE ( 'NONE', *, *, #12273, .T. ) ;
#13423 = CARTESIAN_POINT ( 'NONE',  ( 15.70366306705350112, -0.2717122460102739390, -23.82579074638668004 ) ) ;
#13424 = ORIENTED_EDGE ( 'NONE', *, *, #13860, .T. ) ;
#13425 = AXIS2_PLACEMENT_3D ( 'NONE', #4385, #13918, #6723 ) ;
#13426 = EDGE_CURVE ( 'NONE', #12491, #6308, #10476, .T. ) ;
#13427 = VERTEX_POINT ( 'NONE', #4770 ) ;
#13428 = EDGE_LOOP ( 'NONE', ( #2269, #4172, #11225, #3378 ) ) ;
#13429 = ORIENTED_EDGE ( 'NONE', *, *, #13799, .T. ) ;
#13430 = VERTEX_POINT ( 'NONE', #9486 ) ;
#13431 = AXIS2_PLACEMENT_3D ( 'NONE', #12594, #5537, #6775 ) ;
#13432 = CARTESIAN_POINT ( 'NONE',  ( 15.50000000000000000, 998.9628421096749662, 22.50000000000000000 ) ) ;
#13433 = AXIS2_PLACEMENT_3D ( 'NONE', #3076, #8736, #6435 ) ;
#13434 = EDGE_CURVE ( 'NONE', #3140, #1405, #12475, .T. ) ;
#13435 = PLANE ( 'NONE',  #115 ) ;
#13436 = CARTESIAN_POINT ( 'NONE',  ( -2.115018882620673057, -4.343749999999819700, -3.167137413913937660 ) ) ;
#13437 = DIRECTION ( 'NONE',  ( 0.000000000000000000, -1.000000000000000000, -4.336808689942017736E-16 ) ) ;
#13438 = DIRECTION ( 'NONE',  ( 0.000000000000000000, 4.336808689942017736E-16, -1.000000000000000000 ) ) ;
#13439 = ADVANCED_FACE ( 'NONE', ( #6190 ), #8999, .T. ) ;
#13440 = AXIS2_PLACEMENT_3D ( 'NONE', #12521, #1729, #9871 ) ;
#13441 = EDGE_CURVE ( 'NONE', #11318, #704, #424, .T. ) ;
#13442 = CARTESIAN_POINT ( 'NONE',  ( -15.50000000000000000, -2.500000000000000000, 21.05662432702600029 ) ) ;
#13443 = PLANE ( 'NONE',  #9990 ) ;
#13444 = CARTESIAN_POINT ( 'NONE',  ( -52.77438362644100067, 101.5320169952374414, -147.9984795835769944 ) ) ;
#13445 = CARTESIAN_POINT ( 'NONE',  ( -42.77438362644000591, 110.1741184958670061, -79.59847958357700293 ) ) ;
#13446 = CARTESIAN_POINT ( 'NONE',  ( -65.90140028023257912, 89.17411849586700612, -44.99847958359791988 ) ) ;
#13447 = AXIS2_PLACEMENT_3D ( 'NONE', #3781, #8511, #13257 ) ;
#13448 = ORIENTED_EDGE ( 'NONE', *, *, #13628, .T. ) ;
#13449 = CARTESIAN_POINT ( 'NONE',  ( 21.98164641901421135, -12.60000029085423812, -8.183940086454239093 ) ) ;
#13450 = CIRCLE ( 'NONE', #11206, 8.050000000000000711 ) ;
#13451 = EDGE_LOOP ( 'NONE', ( #13808, #4797, #1224, #5741, #5435, #3885, #9534, #8876 ) ) ;
#13452 = ORIENTED_EDGE ( 'NONE', *, *, #607, .T. ) ;
#13453 = EDGE_LOOP ( 'NONE', ( #11656, #10390, #8844, #11241, #7388, #8686, #13874, #407 ) ) ;
#13454 = CARTESIAN_POINT ( 'NONE',  ( 3.013463120154617148, -5.647500000000105658, -1.249542180252701806 ) ) ;
#13455 =( GEOMETRIC_REPRESENTATION_CONTEXT ( 3 ) GLOBAL_UNCERTAINTY_ASSIGNED_CONTEXT ( ( #13531 ) ) GLOBAL_UNIT_ASSIGNED_CONTEXT ( ( #600, #6375, #3088 ) ) REPRESENTATION_CONTEXT ( 'NONE', 'WORKASPACE' ) );
#13456 = CARTESIAN_POINT ( 'NONE',  ( 0.9404171202240950711, -5.788124999999990195, -3.104336352551607892 ) ) ;
#13457 = LINE ( 'NONE', #5161, #9809 ) ;
#13458 = FACE_OUTER_BOUND ( 'NONE', #13709, .T. ) ;
#13459 = CIRCLE ( 'NONE', #1303, 4.000000000000004441 ) ;
#13460 = CARTESIAN_POINT ( 'NONE',  ( -69.77438362644100778, 82.17411849586699191, -67.49847958357700861 ) ) ;
#13461 = CARTESIAN_POINT ( 'NONE',  ( -53.79538362644100147, 100.9425423703948326, -147.9984795835769944 ) ) ;
#13462 = DIRECTION ( 'NONE',  ( -0.000000000000000000, 1.000000000000000000, -0.000000000000000000 ) ) ;
#13463 = VECTOR ( 'NONE', #2345, 1000.000000000000000 ) ;
#13464 = FACE_OUTER_BOUND ( 'NONE', #17, .T. ) ;
#13465 = ORIENTED_EDGE ( 'NONE', *, *, #277, .T. ) ;
#13466 = CARTESIAN_POINT ( 'NONE',  ( -35.58670980944424400, 5.000000000000001776, 129.5095611191910621 ) ) ;
#13467 = ORIENTED_EDGE ( 'NONE', *, *, #11139, .F. ) ;
#13468 = AXIS2_PLACEMENT_3D ( 'NONE', #4903, #4821, #1546 ) ;
#13469 = DIRECTION ( 'NONE',  ( 1.000000000000000000, 0.000000000000000000, -6.982962677686266711E-15 ) ) ;
#13470 = CARTESIAN_POINT ( 'NONE',  ( 1.163914675889782702, -2.796875000000069722, 3.840555497293599352 ) ) ;
#13471 = EDGE_LOOP ( 'NONE', ( #10731, #7707, #13651, #5820, #14965, #14668 ) ) ;
#13472 = AXIS2_PLACEMENT_3D ( 'NONE', #14744, #1791, #11404 ) ;
#13473 = DIRECTION ( 'NONE',  ( -1.287488025362404182E-15, -1.000000000000000000, 0.000000000000000000 ) ) ;
#13474 = CARTESIAN_POINT ( 'NONE',  ( -13.41835358098579079, -11.75147215343038631, 0.2664120436859898633 ) ) ;
#13475 = DIRECTION ( 'NONE',  ( -0.9961946980917452121, 3.779777825264100874E-17, -0.08715574274766163532 ) ) ;
#13476 = CARTESIAN_POINT ( 'NONE',  ( -15.50000000000000000, -5.000000000000000000, 26.00000000000000000 ) ) ;
#13477 = DIRECTION ( 'NONE',  ( -0.000000000000000000, -0.000000000000000000, 1.000000000000000000 ) ) ;
#13478 = CARTESIAN_POINT ( 'NONE',  ( -0.9013897961777794787, 2.290928418211087614, 4.500000000000000888 ) ) ;
#13479 = CARTESIAN_POINT ( 'NONE',  ( -89.27438362644100778, 110.1741184958670061, -79.59847958357700293 ) ) ;
#13480 = DIRECTION ( 'NONE',  ( 0.000000000000000000, 0.000000000000000000, 1.000000000000000000 ) ) ;
#13481 = CYLINDRICAL_SURFACE ( 'NONE', #4009, 1.000000000000001110 ) ;
#13482 = AXIS2_PLACEMENT_3D ( 'NONE', #14997, #12542, #11368 ) ;
#13483 = ORIENTED_EDGE ( 'NONE', *, *, #5371, .F. ) ;
#13484 = ADVANCED_FACE ( 'NONE', ( #185 ), #7337, .F. ) ;
#13485 = ORIENTED_EDGE ( 'NONE', *, *, #27, .T. ) ;
#13486 = DIRECTION ( 'NONE',  ( -0.9961946980917452121, 3.779777825264100874E-17, -0.08715574274766163532 ) ) ;
#13487 = CARTESIAN_POINT ( 'NONE',  ( 2.100337907687724215, -1.741249999999995968, -3.141606438102673149 ) ) ;
#13488 = ORIENTED_EDGE ( 'NONE', *, *, #6429, .T. ) ;
#13489 = CIRCLE ( 'NONE', #11752, 1.250000000000001110 ) ;
#13490 = EDGE_CURVE ( 'NONE', #3055, #3702, #8272, .T. ) ;
#13491 = VECTOR ( 'NONE', #12247, 1000.000000000000114 ) ;
#13492 = DIRECTION ( 'NONE',  ( 0.000000000000000000, 1.000000000000000000, 0.000000000000000000 ) ) ;
#13493 = FACE_OUTER_BOUND ( 'NONE', #2930, .T. ) ;
#13494 = CARTESIAN_POINT ( 'NONE',  ( -4.763139720814411504, 0.04639863247562014958, -0.7500000000000002220 ) ) ;
#13495 = CARTESIAN_POINT ( 'NONE',  ( -4.296227084909979510, -0.4995677573761841406, -0.01166785054812304046 ) ) ;
#13496 = DIRECTION ( 'NONE',  ( 0.000000000000000000, 0.000000000000000000, 1.000000000000000000 ) ) ;
#13497 = AXIS2_PLACEMENT_3D ( 'NONE', #14329, #7137, #14174 ) ;
#13498 = VECTOR ( 'NONE', #9999, 1000.000000000000000 ) ;
#13499 = AXIS2_PLACEMENT_3D ( 'NONE', #4918, #2422, #9396 ) ;
#13500 = FACE_BOUND ( 'NONE', #10683, .T. ) ;
#13501 = ORIENTED_EDGE ( 'NONE', *, *, #7709, .F. ) ;
#13502 = CARTESIAN_POINT ( 'NONE',  ( 3.469446951953614189E-15, -24.00000000000000000, 6.000000000000000000 ) ) ;
#13503 = ADVANCED_FACE ( 'NONE', ( #8486 ), #5003, .F. ) ;
#13504 = ORIENTED_EDGE ( 'NONE', *, *, #11321, .F. ) ;
#13505 = ORIENTED_EDGE ( 'NONE', *, *, #12388, .F. ) ;
#13506 = VERTEX_POINT ( 'NONE', #9875 ) ;
#13507 = ORIENTED_EDGE ( 'NONE', *, *, #5277, .T. ) ;
#13508 = ORIENTED_EDGE ( 'NONE', *, *, #7820, .T. ) ;
#13509 = FACE_OUTER_BOUND ( 'NONE', #11185, .T. ) ;
#13510 = CARTESIAN_POINT ( 'NONE',  ( -1.439523803302256155, -1.897500000000171383, -3.471712813344601578 ) ) ;
#13511 = DIRECTION ( 'NONE',  ( 9.422394424380278809E-16, -1.000000000000000000, 0.000000000000000000 ) ) ;
#13512 = AXIS2_PLACEMENT_3D ( 'NONE', #13292, #3333, #14881 ) ;
#13513 = CARTESIAN_POINT ( 'NONE',  ( -3.506684959068008034, -4.437500000000057732, -1.453587443624275499 ) ) ;
#13514 = DIRECTION ( 'NONE',  ( 0.000000000000000000, 1.000000000000000000, 0.000000000000000000 ) ) ;
#13515 = DIRECTION ( 'NONE',  ( 0.000000000000000000, -1.000000000000000000, -4.336808689942017736E-16 ) ) ;
#13516 = ADVANCED_FACE ( 'NONE', ( #5230, #11126 ), #13385, .F. ) ;
#13517 = LINE ( 'NONE', #5214, #6656 ) ;
#13518 = CARTESIAN_POINT ( 'NONE',  ( 1.243192046278082774, -0.7968750000001610934, 4.092941397521737912 ) ) ;
#13519 = EDGE_CURVE ( 'NONE', #5033, #13053, #1507, .T. ) ;
#13520 = CARTESIAN_POINT ( 'NONE',  ( -12.81835358098578403, 12.39999970914576188, -9.367156043074160721 ) ) ;
#13521 = PLANE ( 'NONE',  #12290 ) ;
#13522 = DIRECTION ( 'NONE',  ( 0.000000000000000000, 0.000000000000000000, -1.000000000000000000 ) ) ;
#13523 = EDGE_LOOP ( 'NONE', ( #14930, #11590, #3173 ) ) ;
#13524 = FACE_OUTER_BOUND ( 'NONE', #7639, .T. ) ;
#13525 = MECHANICAL_DESIGN_GEOMETRIC_PRESENTATION_REPRESENTATION (  '', ( #14245 ), #10038 ) ;
#13526 = EDGE_CURVE ( 'NONE', #3399, #8984, #11495, .T. ) ;
#13527 = ORIENTED_EDGE ( 'NONE', *, *, #12725, .F. ) ;
#13528 = ORIENTED_EDGE ( 'NONE', *, *, #14404, .T. ) ;
#13529 = ORIENTED_EDGE ( 'NONE', *, *, #2509, .T. ) ;
#13530 = CIRCLE ( 'NONE', #4362, 0.9999999999999994449 ) ;
#13531 = UNCERTAINTY_MEASURE_WITH_UNIT (LENGTH_MEASURE( 1.000000000000000082E-05 ), #600, 'distance_accuracy_value', 'NONE');
#13532 = DIRECTION ( 'NONE',  ( 0.000000000000000000, -1.000000000000000000, 0.000000000000000000 ) ) ;
#13533 = ADVANCED_FACE ( 'NONE', ( #8794 ), #6111, .F. ) ;
#13534 = FACE_OUTER_BOUND ( 'NONE', #4255, .T. ) ;
#13535 = EDGE_CURVE ( 'NONE', #6571, #953, #10972, .T. ) ;
#13536 = CARTESIAN_POINT ( 'NONE',  ( 2.063655046872799215, -5.725624999999673115, -2.513280214060358286 ) ) ;
#13537 = DIRECTION ( 'NONE',  ( -1.000000000000000000, -1.724434379501977811E-15, 0.000000000000000000 ) ) ;
#13538 = CIRCLE ( 'NONE', #11783, 2.042000000000002036 ) ;
#13539 = CARTESIAN_POINT ( 'NONE',  ( -5.196152422706636465, 2.374999999999986677, -8.561039196169309507E-16 ) ) ;
#13540 = CARTESIAN_POINT ( 'NONE',  ( -35.58670980944424400, 5.000000000000001776, 97.50956111919106206 ) ) ;
#13541 = SHAPE_REPRESENTATION ( 'BR-Y-114', ( #2284, #5773, #12452, #4030, #9711, #12206, #7007 ), #7511 ) ;
#13542 = AXIS2_PLACEMENT_3D ( 'NONE', #12458, #4163, #8888 ) ;
#13543 = ADVANCED_FACE ( 'NONE', ( #10821 ), #9642, .T. ) ;
#13544 = DIRECTION ( 'NONE',  ( -1.258331998315348991E-39, 1.000000000000000000, 4.336808689942017243E-16 ) ) ;
#13545 = DIRECTION ( 'NONE',  ( -0.4999999999999832356, 0.000000000000000000, 0.8660254037844483666 ) ) ;
#13546 = VECTOR ( 'NONE', #123, 1000.000000000000000 ) ;
#13547 = DIRECTION ( 'NONE',  ( -1.000000000000000000, 0.000000000000000000, -0.000000000000000000 ) ) ;
#13548 = EDGE_LOOP ( 'NONE', ( #6996, #5550, #12708 ) ) ;
#13549 = DIRECTION ( 'NONE',  ( -1.000000000000000000, 0.000000000000000000, -0.000000000000000000 ) ) ;
#13550 = EDGE_CURVE ( 'NONE', #7940, #8984, #3756, .T. ) ;
#13551 = VECTOR ( 'NONE', #12008, 1000.000000000000000 ) ;
#13552 = CONTEXT_DEPENDENT_SHAPE_REPRESENTATION ( #3263, #163 ) ;
#13553 = EDGE_LOOP ( 'NONE', ( #10016, #8797, #15081, #9364, #2480 ) ) ;
#13554 = CIRCLE ( 'NONE', #3627, 4.250000000000003553 ) ;
#13555 = CARTESIAN_POINT ( 'NONE',  ( -0.001482159116125898214, -2.249999999999994227, -4.085353063378265759 ) ) ;
#13556 = ORIENTED_EDGE ( 'NONE', *, *, #14283, .T. ) ;
#13557 = CIRCLE ( 'NONE', #656, 0.2000000000005261458 ) ;
#13558 = DIRECTION ( 'NONE',  ( 0.000000000000000000, 0.000000000000000000, -1.000000000000000000 ) ) ;
#13559 = LINE ( 'NONE', #7666, #14488 ) ;
#13560 = LINE ( 'NONE', #2840, #60 ) ;
#13561 = CARTESIAN_POINT ( 'NONE',  ( -88.81638362644000040, 63.99516924618178848, -147.9984795835769944 ) ) ;
#13562 = DIRECTION ( 'NONE',  ( 0.000000000000000000, 0.000000000000000000, -1.000000000000000000 ) ) ;
#13563 = CARTESIAN_POINT ( 'NONE',  ( -84.73238362643999722, 66.35306774555222376, -150.4984795835770228 ) ) ;
#13564 = CARTESIAN_POINT ( 'NONE',  ( -86.77438362644001302, 65.17411849586700612, -86.49847958357699440 ) ) ;
#13565 = FACE_OUTER_BOUND ( 'NONE', #8784, .T. ) ;
#13566 = VERTEX_POINT ( 'NONE', #9797 ) ;
#13567 = ORIENTED_EDGE ( 'NONE', *, *, #13797, .F. ) ;
#13568 = CARTESIAN_POINT ( 'NONE',  ( -72.45546847960635262, 74.51466092245016171, -58.65793715699378197 ) ) ;
#13569 = CARTESIAN_POINT ( 'NONE',  ( -0.3703630857573827484, -1.850625000000086562, -3.746264557426809638 ) ) ;
#13570 = VERTEX_POINT ( 'NONE', #3912 ) ;
#13571 = CIRCLE ( 'NONE', #3396, 0.5999999999999998668 ) ;
#13572 = CARTESIAN_POINT ( 'NONE',  ( -55.27438362644100067, 99.17411849586700612, -182.2484795835770228 ) ) ;
#13573 = DIRECTION ( 'NONE',  ( -0.9961946980917453232, 7.200509705930738460E-17, -0.08715574274766157981 ) ) ;
#13574 = CYLINDRICAL_SURFACE ( 'NONE', #3317, 0.9999999999999994449 ) ;
#13575 = CARTESIAN_POINT ( 'NONE',  ( 3.558919284812731565, -0.4995676945082496712, -1.914344080127182268 ) ) ;
#13576 = CARTESIAN_POINT ( 'NONE',  ( 17.18164641901421419, 11.39999970914576011, 0.8664120436859875651 ) ) ;
#13577 = EDGE_CURVE ( 'NONE', #3702, #3055, #6554, .T. ) ;
#13578 = FACE_OUTER_BOUND ( 'NONE', #2390, .T. ) ;
#13579 = CONICAL_SURFACE ( 'NONE', #6890, 2.042000000000002036, 1.047197551196596965 ) ;
#13580 = EDGE_LOOP ( 'NONE', ( #9289, #12340, #3652, #8861 ) ) ;
#13581 = CARTESIAN_POINT ( 'NONE',  ( -35.58670980944424400, 2.488961461112888074, 129.5095611191910621 ) ) ;
#13582 = VERTEX_POINT ( 'NONE', #7494 ) ;
#13583 = EDGE_LOOP ( 'NONE', ( #10199, #3238, #3632, #229, #6137 ) ) ;
#13584 = EDGE_LOOP ( 'NONE', ( #3767, #7211, #1770, #2715, #2869 ) ) ;
#13585 = ORIENTED_EDGE ( 'NONE', *, *, #13960, .F. ) ;
#13586 = EDGE_LOOP ( 'NONE', ( #5388, #7677 ) ) ;
#13587 = LINE ( 'NONE', #542, #12504 ) ;
#13588 = AXIS2_PLACEMENT_3D ( 'NONE', #3564, #2469, #7070 ) ;
#13589 = CARTESIAN_POINT ( 'NONE',  ( -2.598076211353321341, 2.374999999999993339, -4.499999999999999112 ) ) ;
#13590 = CARTESIAN_POINT ( 'NONE',  ( -1.775679308629948050, -4.671875000000182077, 3.319983975552966537 ) ) ;
#13591 = CARTESIAN_POINT ( 'NONE',  ( -9.797174393178927223E-17, 9.500000000000000000, 0.000000000000000000 ) ) ;
#13592 = EDGE_CURVE ( 'NONE', #5341, #1220, #14459, .T. ) ;
#13593 = LINE ( 'NONE', #12506, #2901 ) ;
#13594 = CARTESIAN_POINT ( 'NONE',  ( -86.77438362643999881, 67.53201699523744139, -150.4984795835770228 ) ) ;
#13595 = CARTESIAN_POINT ( 'NONE',  ( -0.8118119174735605181, -1.718749999999964917, 4.075604227461077755 ) ) ;
#13596 = CARTESIAN_POINT ( 'NONE',  ( -79.02077156573416516, 60.67411849586702743, -152.4984795835769944 ) ) ;
#13597 = FACE_OUTER_BOUND ( 'NONE', #7206, .T. ) ;
#13598 = EDGE_CURVE ( 'NONE', #2303, #8186, #1590, .T. ) ;
#13599 = CARTESIAN_POINT ( 'NONE',  ( 16.74999999999999289, -0.3152037684892571301, 22.25410949791978155 ) ) ;
#13600 = EDGE_LOOP ( 'NONE', ( #9411, #9633 ) ) ;
#13601 = DIRECTION ( 'NONE',  ( 1.000000000000000000, 0.000000000000000000, 0.000000000000000000 ) ) ;
#13602 = ORIENTED_EDGE ( 'NONE', *, *, #4798, .T. ) ;
#13603 = ORIENTED_EDGE ( 'NONE', *, *, #13592, .T. ) ;
#13604 = ORIENTED_EDGE ( 'NONE', *, *, #1762, .F. ) ;
#13605 = CARTESIAN_POINT ( 'NONE',  ( 57.41329019055577021, 5.000000000000000000, 97.50956111919106206 ) ) ;
#13606 = CARTESIAN_POINT ( 'NONE',  ( -1.562933739280453205, -5.256875000000181153, 2.922265072135110220 ) ) ;
#13607 = DIRECTION ( 'NONE',  ( 0.8660254037844387076, 0.4999999999999998890, 0.000000000000000000 ) ) ;
#13608 = CARTESIAN_POINT ( 'NONE',  ( -1.673688575075004152E-15, 4.650702586819541295, 0.000000000000000000 ) ) ;
#13609 = ADVANCED_FACE ( 'NONE', ( #5628 ), #10489, .F. ) ;
#13610 = LINE ( 'NONE', #2978, #13770 ) ;
#13611 = DIRECTION ( 'NONE',  ( -0.8660254037844381525, 0.000000000000000000, -0.5000000000000007772 ) ) ;
#13612 = LINE ( 'NONE', #3205, #12243 ) ;
#13613 = EDGE_CURVE ( 'NONE', #11082, #8835, #7616, .T. ) ;
#13614 = CARTESIAN_POINT ( 'NONE',  ( 1.208453367980061088, -5.394866591894509789, 3.060934444180607450 ) ) ;
#13615 = EDGE_CURVE ( 'NONE', #9681, #4480, #11743, .T. ) ;
#13616 = ORIENTED_EDGE ( 'NONE', *, *, #8833, .T. ) ;
#13617 = FACE_OUTER_BOUND ( 'NONE', #14887, .T. ) ;
#13618 = ORIENTED_EDGE ( 'NONE', *, *, #6578, .F. ) ;
#13619 = CARTESIAN_POINT ( 'NONE',  ( 21.98164641901421135, 11.99999970914576686, -14.73358795631400575 ) ) ;
#13620 = ADVANCED_FACE ( 'NONE', ( #644 ), #15057, .F. ) ;
#13621 = CARTESIAN_POINT ( 'NONE',  ( 3.905735209131758534, -3.031249999999969802, -0.7758307200683374205 ) ) ;
#13622 = ORIENTED_EDGE ( 'NONE', *, *, #4800, .T. ) ;
#13623 = CARTESIAN_POINT ( 'NONE',  ( -0.001018162134759268388, -3.749213562372953223, 3.887570876297712363 ) ) ;
#13624 = CARTESIAN_POINT ( 'NONE',  ( -84.73238362643999722, 66.35306774555222376, -147.9984795835769944 ) ) ;
#13625 = EDGE_CURVE ( 'NONE', #11570, #5237, #13612, .T. ) ;
#13626 = DIRECTION ( 'NONE',  ( 0.000000000000000000, 0.000000000000000000, -1.000000000000000000 ) ) ;
#13627 = CARTESIAN_POINT ( 'NONE',  ( 1.732658076282566739, 0.04645217140505895209, -4.499999999999999112 ) ) ;
#13628 = EDGE_CURVE ( 'NONE', #4013, #5361, #1079, .T. ) ;
#13629 = DIRECTION ( 'NONE',  ( 0.000000000000000000, -1.000000000000000000, 0.000000000000000000 ) ) ;
#13630 = EDGE_CURVE ( 'NONE', #4633, #13125, #11485, .T. ) ;
#13631 = CARTESIAN_POINT ( 'NONE',  ( -1.770063184917655574, 2.057215485424180201, 4.500000000000000888 ) ) ;
#13632 = DIRECTION ( 'NONE',  ( 1.000000000000000000, -0.000000000000000000, 1.224646799147353207E-16 ) ) ;
#13633 = CARTESIAN_POINT ( 'NONE',  ( -70.06129951035623549, 98.17413497942138179, -94.70806078951538609 ) ) ;
#13634 = DIRECTION ( 'NONE',  ( 0.000000000000000000, 0.000000000000000000, 1.000000000000000000 ) ) ;
#13635 = ORIENTED_EDGE ( 'NONE', *, *, #6508, .T. ) ;
#13636 = DIRECTION ( 'NONE',  ( 0.000000000000000000, 0.000000000000000000, 1.000000000000000000 ) ) ;
#13637 = ORIENTED_EDGE ( 'NONE', *, *, #4021, .F. ) ;
#13638 = LINE ( 'NONE', #12471, #2858 ) ;
#13639 = CARTESIAN_POINT ( 'NONE',  ( 2.123627735229572266, -1.428750000000023501, 3.175715285003386956 ) ) ;
#13640 = ORIENTED_EDGE ( 'NONE', *, *, #6216, .T. ) ;
#13641 = LINE ( 'NONE', #4401, #12911 ) ;
#13642 = PRODUCT_DEFINITION_SHAPE ( 'NONE', 'NONE',  #15339 ) ;
#13643 = CARTESIAN_POINT ( 'NONE',  ( -1.673688575075004152E-15, 4.650702586819541295, 0.000000000000000000 ) ) ;
#13644 = CARTESIAN_POINT ( 'NONE',  ( 17.21739630941073429, -3.630123888347186245, 0.07286771090926238981 ) ) ;
#13645 = CARTESIAN_POINT ( 'NONE',  ( -4.091800360845128992, -0.4995676945082698217, -1.248354756450685832 ) ) ;
#13646 = PLANE ( 'NONE',  #10796 ) ;
#13647 = DIRECTION ( 'NONE',  ( 0.000000000000000000, 0.000000000000000000, -1.000000000000000000 ) ) ;
#13648 = ORIENTED_EDGE ( 'NONE', *, *, #10649, .T. ) ;
#13649 = FACE_OUTER_BOUND ( 'NONE', #7386, .T. ) ;
#13650 = ORIENTED_EDGE ( 'NONE', *, *, #1666, .F. ) ;
#13651 = ORIENTED_EDGE ( 'NONE', *, *, #1373, .T. ) ;
#13652 = VERTEX_POINT ( 'NONE', #11278 ) ;
#13653 = VERTEX_POINT ( 'NONE', #12665 ) ;
#13654 = ORIENTED_EDGE ( 'NONE', *, *, #6046, .T. ) ;
#13655 = CARTESIAN_POINT ( 'NONE',  ( 0.3539834606289790075, -5.764838562372911923, 3.603588891846962738 ) ) ;
#13656 = CARTESIAN_POINT ( 'NONE',  ( -3.284049251726958829, -2.163124999999908482, 1.754264853118110423 ) ) ;
#13657 = CARTESIAN_POINT ( 'NONE',  ( -15.50000000000000000, -1.037157890325000054, -22.50000000000000000 ) ) ;
#13658 = CARTESIAN_POINT ( 'NONE',  ( 3.820852842225918700, -2.953124999999806821, 1.157524667501716786 ) ) ;
#13659 = CARTESIAN_POINT ( 'NONE',  ( -16.75000000000000000, -0.3156864504677194816, 22.25638000318209109 ) ) ;
#13660 = LINE ( 'NONE', #765, #2148 ) ;
#13661 = LINE ( 'NONE', #6464, #7407 ) ;
#13662 = CARTESIAN_POINT ( 'NONE',  ( -4.100362740845592491, -1.531249999999860556, 0.8144810970459482879 ) ) ;
#13663 = FACE_BOUND ( 'NONE', #297, .T. ) ;
#13664 = LINE ( 'NONE', #9858, #7836 ) ;
#13665 = DIRECTION ( 'NONE',  ( 0.000000000000000000, 0.000000000000000000, 1.000000000000000000 ) ) ;
#13666 = AXIS2_PLACEMENT_3D ( 'NONE', #8579, #5968, #9577 ) ;
#13667 = EDGE_LOOP ( 'NONE', ( #4058, #5136, #11781, #1044 ) ) ;
#13668 = CARTESIAN_POINT ( 'NONE',  ( -57.02438362643999170, 65.17411849586700612, -145.4984795835769660 ) ) ;
#13669 = ORIENTED_EDGE ( 'NONE', *, *, #3538, .T. ) ;
#13670 = AXIS2_PLACEMENT_3D ( 'NONE', #5708, #10406, #13078 ) ;
#13671 = EDGE_LOOP ( 'NONE', ( #2949, #688, #2444, #11182 ) ) ;
#13672 = EDGE_LOOP ( 'NONE', ( #15060, #11550 ) ) ;
#13673 = EDGE_CURVE ( 'NONE', #4034, #8371, #13160, .T. ) ;
#13674 = ADVANCED_BREP_SHAPE_REPRESENTATION ( '', ( #5480, #357, #418, #285 ), #15141 ) ;
#13675 = LINE ( 'NONE', #10322, #14667 ) ;
#13676 = CARTESIAN_POINT ( 'NONE',  ( 2.085982869228583780, -5.444374999999953779, 2.543086608318696928 ) ) ;
#13677 = EDGE_CURVE ( 'NONE', #3401, #14989, #4549, .T. ) ;
#13678 = AXIS2_PLACEMENT_3D ( 'NONE', #8022, #5644, #9031 ) ;
#13679 = CARTESIAN_POINT ( 'NONE',  ( -54.81638362644000040, 66.35306774555222376, -147.9984795835769944 ) ) ;
#13680 = LINE ( 'NONE', #5079, #1521 ) ;
#13681 = CARTESIAN_POINT ( 'NONE',  ( -2.598076211353316012, 0.1227504548087343245, -4.499999999999999112 ) ) ;
#13682 = CARTESIAN_POINT ( 'NONE',  ( -90.85838362644101096, 99.17411849586700612, -147.9984795835769944 ) ) ;
#13683 = CARTESIAN_POINT ( 'NONE',  ( 1.151041666666722030, 7.362500000000001599, 0.000000000000000000 ) ) ;
#13684 = CARTESIAN_POINT ( 'NONE',  ( -3.186695398571379290, -5.131874999999967990, 0.9679749472946410638 ) ) ;
#13685 = VERTEX_POINT ( 'NONE', #7167 ) ;
#13686 = CARTESIAN_POINT ( 'NONE',  ( -86.77438362644100778, 101.5320169952374414, -150.4984795835770228 ) ) ;
#13687 = ORIENTED_EDGE ( 'NONE', *, *, #7712, .F. ) ;
#13688 = AXIS2_PLACEMENT_3D ( 'NONE', #5623, #14897, #4286 ) ;
#13689 = CONTEXT_DEPENDENT_SHAPE_REPRESENTATION ( #10392, #6348 ) ;
#13690 = ADVANCED_FACE ( 'NONE', ( #9241 ), #6932, .T. ) ;
#13691 = ORIENTED_EDGE ( 'NONE', *, *, #11256, .F. ) ;
#13692 = CARTESIAN_POINT ( 'NONE',  ( -3.563986660466321510, -2.578124999999990230, 1.906655726273616125 ) ) ;
#13693 = ORIENTED_EDGE ( 'NONE', *, *, #9252, .T. ) ;
#13694 = AXIS2_PLACEMENT_3D ( 'NONE', #7315, #10714, #10800 ) ;
#13695 = EDGE_CURVE ( 'NONE', #13506, #5739, #12489, .T. ) ;
#13696 = DIRECTION ( 'NONE',  ( 0.000000000000000000, 1.000000000000000000, 0.000000000000000000 ) ) ;
#13697 = FACE_BOUND ( 'NONE', #4339, .T. ) ;
#13698 = CARTESIAN_POINT ( 'NONE',  ( -64.53565528768383786, 67.29799558322736175, -83.44847958357698303 ) ) ;
#13699 = EDGE_CURVE ( 'NONE', #8210, #5814, #9249, .T. ) ;
#13700 = CARTESIAN_POINT ( 'NONE',  ( -88.81638362644000040, 63.99516924618178848, -147.9984795835769944 ) ) ;
#13701 = CARTESIAN_POINT ( 'NONE',  ( 2.598076211353311127, 1.678847577293378190, 4.500000000000000000 ) ) ;
#13702 = EDGE_CURVE ( 'NONE', #7247, #8682, #944, .T. ) ;
#13703 = CARTESIAN_POINT ( 'NONE',  ( 0.8000000000000123679, 8.384405323238834029, 9.797174393178965434E-17 ) ) ;
#13704 = LINE ( 'NONE', #1751, #2899 ) ;
#13705 = AXIS2_PLACEMENT_3D ( 'NONE', #7587, #7509, #12313 ) ;
#13706 = AXIS2_PLACEMENT_3D ( 'NONE', #12808, #5612, #10318 ) ;
#13707 = LINE ( 'NONE', #8894, #3025 ) ;
#13708 = EDGE_CURVE ( 'NONE', #4222, #11928, #2425, .T. ) ;
#13709 = EDGE_LOOP ( 'NONE', ( #7406, #15026, #14592, #320 ) ) ;
#13710 = CIRCLE ( 'NONE', #2548, 4.249999999999996447 ) ;
#13711 = CARTESIAN_POINT ( 'NONE',  ( -52.77438362643999881, 65.17411849586700612, -182.2484795835770228 ) ) ;
#13712 = CARTESIAN_POINT ( 'NONE',  ( -1.470831194960215083, -1.272500000000085230, 3.548278161707651535 ) ) ;
#13713 = ORIENTED_EDGE ( 'NONE', *, *, #12258, .T. ) ;
#13714 = EDGE_CURVE ( 'NONE', #14839, #3939, #4750, .T. ) ;
#13715 = DIRECTION ( 'NONE',  ( 0.000000000000000000, 1.000000000000000000, 0.000000000000000000 ) ) ;
#13716 = VECTOR ( 'NONE', #1793, 1000.000000000000114 ) ;
#13717 = CARTESIAN_POINT ( 'NONE',  ( -56.85838362643999488, 65.17411849586700612, -147.9984795835769944 ) ) ;
#13718 = VECTOR ( 'NONE', #12426, 1000.000000000000000 ) ;
#13719 = CARTESIAN_POINT ( 'NONE',  ( -13.41835358098578723, -2.908542394189813650E-07, 0.2664120436859911956 ) ) ;
#13720 = DIRECTION ( 'NONE',  ( 0.8660254037844485886, 0.000000000000000000, -0.4999999999999827360 ) ) ;
#13721 = DIRECTION ( 'NONE',  ( 0.000000000000000000, 1.000000000000000000, 4.336808689942017736E-16 ) ) ;
#13722 = FACE_OUTER_BOUND ( 'NONE', #15216, .T. ) ;
#13723 = VERTEX_POINT ( 'NONE', #4682 ) ;
#13724 = DIRECTION ( 'NONE',  ( -1.000000000000000000, 0.000000000000000000, 0.000000000000000000 ) ) ;
#13725 = VECTOR ( 'NONE', #10803, 1000.000000000000000 ) ;
#13726 = AXIS2_PLACEMENT_3D ( 'NONE', #13356, #2714, #3799 ) ;
#13727 = ADVANCED_FACE ( 'NONE', ( #9395 ), #9321, .T. ) ;
#13728 = VERTEX_POINT ( 'NONE', #14291 ) ;
#13729 = VERTEX_POINT ( 'NONE', #12823 ) ;
#13730 = ORIENTED_EDGE ( 'NONE', *, *, #1755, .F. ) ;
#13731 = ORIENTED_EDGE ( 'NONE', *, *, #9578, .T. ) ;
#13732 = ORIENTED_EDGE ( 'NONE', *, *, #1470, .T. ) ;
#13733 = CARTESIAN_POINT ( 'NONE',  ( 2.288508625327937640, -5.858588562373046926, 2.790022829016634454 ) ) ;
#13734 = CARTESIAN_POINT ( 'NONE',  ( 3.931950937192209228, -0.5849999999998678479, -0.001434051515494208940 ) ) ;
#13735 = DIRECTION ( 'NONE',  ( 0.000000000000000000, 0.000000000000000000, 1.000000000000000000 ) ) ;
#13736 = CARTESIAN_POINT ( 'NONE',  ( 2.515861257320511246, -3.140624999999957367, -3.067863912704874796 ) ) ;
#13737 = VECTOR ( 'NONE', #1690, 1000.000000000000114 ) ;
#13738 = CARTESIAN_POINT ( 'NONE',  ( -50.73238362644099197, 100.3530677455522238, -150.4984795835770228 ) ) ;
#13739 = AXIS2_PLACEMENT_3D ( 'NONE', #1988, #6671, #11156 ) ;
#13740 = DIRECTION ( 'NONE',  ( 1.000000000000000000, 0.000000000000000000, 0.000000000000000000 ) ) ;
#13741 = DIRECTION ( 'NONE',  ( -0.9961946980917452121, 3.779777825264100874E-17, -0.08715574274766163532 ) ) ;
#13742 = CARTESIAN_POINT ( 'NONE',  ( 4.228334800557012940, -1.015625000000088818, -0.4153177470898732904 ) ) ;
#13743 = CARTESIAN_POINT ( 'NONE',  ( 0.000000000000000000, 0.000000000000000000, 0.000000000000000000 ) ) ;
#13744 = DIRECTION ( 'NONE',  ( 1.000000000000000000, 0.000000000000000000, 0.000000000000000000 ) ) ;
#13745 = CARTESIAN_POINT ( 'NONE',  ( 16.75000000000000000, -0.2038245569916320166, 21.77831216351300014 ) ) ;
#13746 = ORIENTED_EDGE ( 'NONE', *, *, #6161, .F. ) ;
#13747 = LINE ( 'NONE', #3117, #10478 ) ;
#13748 = ORIENTED_EDGE ( 'NONE', *, *, #10473, .F. ) ;
#13749 = ORIENTED_EDGE ( 'NONE', *, *, #7568, .T. ) ;
#13750 = ORIENTED_EDGE ( 'NONE', *, *, #14503, .F. ) ;
#13751 = VECTOR ( 'NONE', #2188, 1000.000000000000000 ) ;
#13752 = CARTESIAN_POINT ( 'NONE',  ( -22.96690797774568082, 1.660051434983101380E-15, 52.36213013816526285 ) ) ;
#13753 = CARTESIAN_POINT ( 'NONE',  ( -0.6836773592642079178, -3.866249999999994635, -3.430425219284937821 ) ) ;
#13754 = DIRECTION ( 'NONE',  ( 0.000000000000000000, 0.000000000000000000, 1.000000000000000000 ) ) ;
#13755 = CARTESIAN_POINT ( 'NONE',  ( 57.41329019055577021, 5.000000000000000000, 131.2954986191910791 ) ) ;
#13756 = CARTESIAN_POINT ( 'NONE',  ( -69.77438362644001302, 82.17411849586700612, -150.4984795835769944 ) ) ;
#13757 = CARTESIAN_POINT ( 'NONE',  ( -69.77438362644001302, 82.17411849586700612, -85.04847958357700577 ) ) ;
#13758 = DIRECTION ( 'NONE',  ( -1.000000000000000000, 0.000000000000000000, 0.000000000000000000 ) ) ;
#13759 = CARTESIAN_POINT ( 'NONE',  ( -69.77438362644001302, 74.17411849586699191, -58.99847958357700151 ) ) ;
#13760 = CARTESIAN_POINT ( 'NONE',  ( -3.268702447147800783, -5.116250000000009734, 0.6493246907702930892 ) ) ;
#13761 = ORIENTED_EDGE ( 'NONE', *, *, #1435, .T. ) ;
#13762 = CIRCLE ( 'NONE', #14491, 0.9999999999999994449 ) ;
#13763 = CARTESIAN_POINT ( 'NONE',  ( 57.41329019055577021, 5.000000000000000000, 129.5095611191910621 ) ) ;
#13764 = EDGE_CURVE ( 'NONE', #12943, #7936, #4521, .T. ) ;
#13765 = VERTEX_POINT ( 'NONE', #8240 ) ;
#13766 = LINE ( 'NONE', #5477, #14146 ) ;
#13767 = EDGE_LOOP ( 'NONE', ( #2559, #13527, #909, #11246 ) ) ;
#13768 = CARTESIAN_POINT ( 'NONE',  ( -2.335396930795095471, -1.343749999999818368, -3.497180482087419051 ) ) ;
#13769 = ORIENTED_EDGE ( 'NONE', *, *, #2677, .F. ) ;
#13770 = VECTOR ( 'NONE', #9944, 1000.000000000000114 ) ;
#13771 = FACE_OUTER_BOUND ( 'NONE', #3641, .T. ) ;
#13772 = CARTESIAN_POINT ( 'NONE',  ( -52.77438362644000591, 99.17411849586700612, -145.4984795835769660 ) ) ;
#13773 = LINE ( 'NONE', #14921, #2309 ) ;
#13774 = PRODUCT_DEFINITION ( 'UNKNOWN', '', #6453, #4060 ) ;
#13775 = EDGE_CURVE ( 'NONE', #14091, #12096, #6313, .T. ) ;
#13776 = CYLINDRICAL_SURFACE ( 'NONE', #6196, 4.500000000000003553 ) ;
#13777 = CARTESIAN_POINT ( 'NONE',  ( -69.77438362644001302, 82.17411849586700612, -85.04847958357699156 ) ) ;
#13778 = DIRECTION ( 'NONE',  ( 0.000000000000000000, 0.000000000000000000, -1.000000000000000000 ) ) ;
#13779 = CIRCLE ( 'NONE', #2134, 4.000000000000000000 ) ;
#13780 = DIRECTION ( 'NONE',  ( -1.000000000000000000, 0.000000000000000000, 0.000000000000000000 ) ) ;
#13781 = EDGE_CURVE ( 'NONE', #13263, #2616, #14062, .T. ) ;
#13782 = CARTESIAN_POINT ( 'NONE',  ( -86.77438362644100778, 99.17411849586700612, -147.9984795835769944 ) ) ;
#13783 = CIRCLE ( 'NONE', #6370, 0.8600000000000014300 ) ;
#13784 = AXIS2_PLACEMENT_3D ( 'NONE', #7645, #2585, #12289 ) ;
#13785 = ORIENTED_EDGE ( 'NONE', *, *, #5456, .F. ) ;
#13786 = CARTESIAN_POINT ( 'NONE',  ( -52.77438362644100067, 96.81621999649657084, -147.9984795835769944 ) ) ;
#13787 = CARTESIAN_POINT ( 'NONE',  ( -1.872693635133553691, -0.2568750000000157852, 3.506634376076540160 ) ) ;
#13788 = ORIENTED_EDGE ( 'NONE', *, *, #9898, .F. ) ;
#13789 = ADVANCED_FACE ( 'NONE', ( #14208 ), #2343, .T. ) ;
#13790 = AXIS2_PLACEMENT_3D ( 'NONE', #8568, #7498, #14310 ) ;
#13791 = TOROIDAL_SURFACE ( 'NONE', #5395, 3.299999999999474909, 0.2000000000005234813 ) ;
#13792 = DIRECTION ( 'NONE',  ( 0.8660254037844381525, 1.060575238724905436E-16, -0.5000000000000007772 ) ) ;
#13793 = EDGE_CURVE ( 'NONE', #6998, #957, #12743, .T. ) ;
#13794 = DIRECTION ( 'NONE',  ( 0.000000000000000000, 0.000000000000000000, -1.000000000000000000 ) ) ;
#13795 = PRESENTATION_STYLE_ASSIGNMENT (( #8751 ) ) ;
#13796 = DIRECTION ( 'NONE',  ( 0.000000000000000000, 1.000000000000000000, 0.000000000000000000 ) ) ;
#13797 = EDGE_CURVE ( 'NONE', #6270, #8132, #10014, .T. ) ;
#13798 = DIRECTION ( 'NONE',  ( 0.000000000000000000, 0.000000000000000000, 1.000000000000000000 ) ) ;
#13799 = EDGE_CURVE ( 'NONE', #856, #11545, #10, .T. ) ;
#13800 = ORIENTED_EDGE ( 'NONE', *, *, #6044, .T. ) ;
#13801 = CARTESIAN_POINT ( 'NONE',  ( -91.27438362643999881, 65.17411849586700612, -86.49847958357699440 ) ) ;
#13802 = AXIS2_PLACEMENT_3D ( 'NONE', #12197, #9861, #13373 ) ;
#13803 = ORIENTED_EDGE ( 'NONE', *, *, #4136, .F. ) ;
#13804 = AXIS2_PLACEMENT_3D ( 'NONE', #5500, #5581, #10282 ) ;
#13805 = ORIENTED_EDGE ( 'NONE', *, *, #10190, .T. ) ;
#13806 = ORIENTED_EDGE ( 'NONE', *, *, #14503, .T. ) ;
#13807 = ORIENTED_EDGE ( 'NONE', *, *, #1726, .F. ) ;
#13808 = ORIENTED_EDGE ( 'NONE', *, *, #4236, .T. ) ;
#13809 = CARTESIAN_POINT ( 'NONE',  ( -1.388373139153629587, -5.686713562372827546, 3.355330185783546249 ) ) ;
#13810 = EDGE_CURVE ( 'NONE', #4506, #12668, #13234, .T. ) ;
#13811 = CARTESIAN_POINT ( 'NONE',  ( -3.844997831300932756, -1.100624999999974429, 0.3801187285354425405 ) ) ;
#13812 = FACE_OUTER_BOUND ( 'NONE', #2986, .T. ) ;
#13813 = CARTESIAN_POINT ( 'NONE',  ( -3.752022838101215285, -2.437499999999895195, -1.552542887664947635 ) ) ;
#13814 = DIRECTION ( 'NONE',  ( 1.060575238724892987E-16, 0.5000000000000199840, -0.8660254037844271613 ) ) ;
#13815 = EDGE_CURVE ( 'NONE', #6563, #13238, #12061, .T. ) ;
#13816 = DIRECTION ( 'NONE',  ( 1.000000000000000000, 0.000000000000000000, 0.000000000000000000 ) ) ;
#13817 = VECTOR ( 'NONE', #10561, 1000.000000000000000 ) ;
#13818 = CARTESIAN_POINT ( 'NONE',  ( -86.77438362644001302, 65.17411849586700612, -145.4984795835769660 ) ) ;
#13819 = CARTESIAN_POINT ( 'NONE',  ( -2.948053448091068507, -1.625000000000079936, 2.946489148067756858 ) ) ;
#13820 = DIRECTION ( 'NONE',  ( -1.000000000000000000, 0.000000000000000000, 0.000000000000000000 ) ) ;
#13821 = CARTESIAN_POINT ( 'NONE',  ( 15.70313394608856683, -0.2715358723588608414, -21.17390376548178210 ) ) ;
#13822 = CARTESIAN_POINT ( 'NONE',  ( -15.70366306705059323, -0.2717122460101009662, -21.17420925361163953 ) ) ;
#13823 = ORIENTED_EDGE ( 'NONE', *, *, #4762, .F. ) ;
#13824 = DIRECTION ( 'NONE',  ( 1.000000000000000000, 0.000000000000000000, 0.000000000000000000 ) ) ;
#13825 = ORIENTED_EDGE ( 'NONE', *, *, #12101, .F. ) ;
#13826 = VERTEX_POINT ( 'NONE', #12123 ) ;
#13827 = ORIENTED_EDGE ( 'NONE', *, *, #12957, .T. ) ;
#13828 = VECTOR ( 'NONE', #10950, 1000.000000000000000 ) ;
#13829 = FACE_OUTER_BOUND ( 'NONE', #4689, .T. ) ;
#13830 = CARTESIAN_POINT ( 'NONE',  ( 0.9808155824294413350, -4.788124999999903153, -3.230360883553721862 ) ) ;
#13831 = LINE ( 'NONE', #2030, #11556 ) ;
#13832 = LINE ( 'NONE', #1959, #14661 ) ;
#13833 = DIRECTION ( 'NONE',  ( 1.000000000000000000, 0.000000000000000000, 0.000000000000000000 ) ) ;
#13834 = CARTESIAN_POINT ( 'NONE',  ( -69.77438362644001302, 74.17411849586699191, -58.99847958357700151 ) ) ;
#13835 = DIRECTION ( 'NONE',  ( 1.000000000000000000, 0.000000000000000000, 0.000000000000000000 ) ) ;
#13836 = CARTESIAN_POINT ( 'NONE',  ( 16.75000000000000000, -2.500000000000000000, -21.77831216351300014 ) ) ;
#13837 = CIRCLE ( 'NONE', #9863, 4.500000000000003553 ) ;
#13838 = VERTEX_POINT ( 'NONE', #1493 ) ;
#13839 = CARTESIAN_POINT ( 'NONE',  ( 2.573385150445058223, -19.31989681812820692, 6.000000000000000000 ) ) ;
#13840 = VERTEX_POINT ( 'NONE', #11962 ) ;
#13841 = LINE ( 'NONE', #10488, #2496 ) ;
#13842 = ORIENTED_EDGE ( 'NONE', *, *, #12853, .F. ) ;
#13843 = CARTESIAN_POINT ( 'NONE',  ( 4.228334800557012940, -1.015625000000088818, -0.4153177470898732904 ) ) ;
#13844 = ORIENTED_EDGE ( 'NONE', *, *, #7611, .F. ) ;
#13845 = CARTESIAN_POINT ( 'NONE',  ( 3.965348895242338134, -3.014838562373144182, -0.3920103835965588757 ) ) ;
#13846 = VECTOR ( 'NONE', #10840, 999.9999999999998863 ) ;
#13847 = LINE ( 'NONE', #15070, #6992 ) ;
#13848 = EDGE_CURVE ( 'NONE', #2616, #6604, #8517, .T. ) ;
#13849 = DIRECTION ( 'NONE',  ( 0.000000000000000000, 1.000000000000000000, 0.000000000000000000 ) ) ;
#13850 = CARTESIAN_POINT ( 'NONE',  ( 15.50000000000000000, -5.000000000000000000, 22.50000000000000000 ) ) ;
#13851 = CARTESIAN_POINT ( 'NONE',  ( -80.52077156573417938, 103.6741184958669777, -152.4984795835769944 ) ) ;
#13852 = CARTESIAN_POINT ( 'NONE',  ( -31.00000000000000000, -2.500000000000000000, 45.00000000000000000 ) ) ;
#13853 = ORIENTED_EDGE ( 'NONE', *, *, #2193, .T. ) ;
#13854 = SURFACE_STYLE_USAGE ( .BOTH. , #7953 ) ;
#13855 = CARTESIAN_POINT ( 'NONE',  ( -2.595824455272694564, -5.375000000000100364, -2.597168749630690332 ) ) ;
#13856 = VERTEX_POINT ( 'NONE', #8695 ) ;
#13857 = EDGE_CURVE ( 'NONE', #10251, #12753, #11029, .T. ) ;
#13858 = CARTESIAN_POINT ( 'NONE',  ( 3.503209385669602938, -1.647500000000019948, -1.450007420588620866 ) ) ;
#13859 = CARTESIAN_POINT ( 'NONE',  ( -0.8655643756568760505, -2.519089588807311881E-15, -4.499999999999999112 ) ) ;
#13860 = EDGE_CURVE ( 'NONE', #9916, #12014, #5215, .T. ) ;
#13861 = B_SPLINE_CURVE_WITH_KNOTS ( 'NONE', 3,
 ( #8391, #5, #76, #7088, #2182, #11645 ),
 .UNSPECIFIED., .F., .F.,
 ( 4, 2, 4 ),
 ( 0.0002380763768129734448, 0.7291065797294589146, 1.457975083082104995 ),
 .UNSPECIFIED. ) ;
#13862 = CARTESIAN_POINT ( 'NONE',  ( -82.27438362643999881, 65.17411849586700612, -145.4984795835769660 ) ) ;
#13863 = CARTESIAN_POINT ( 'NONE',  ( 3.372444421885775423, -0.4995676945082423992, 2.006840812041871924 ) ) ;
#13864 = CARTESIAN_POINT ( 'NONE',  ( 1.592763020438999089, -1.151251418009690488E-16, 0.1393487079717274646 ) ) ;
#13865 = CARTESIAN_POINT ( 'NONE',  ( 57.41329019055577021, 0.000000000000000000, 97.50956111919106206 ) ) ;
#13866 = CARTESIAN_POINT ( 'NONE',  ( -3.081487911019577365E-30, 0.000000000000000000, 0.000000000000000000 ) ) ;
#13867 = VERTEX_POINT ( 'NONE', #2802 ) ;
#13868 = CARTESIAN_POINT ( 'NONE',  ( -2.598076211353315568, 0.1227504548087345604, 4.500000000000000888 ) ) ;
#13869 = ORIENTED_EDGE ( 'NONE', *, *, #7611, .T. ) ;
#13870 = VERTEX_POINT ( 'NONE', #5147 ) ;
#13871 = VERTEX_POINT ( 'NONE', #310 ) ;
#13872 = ORIENTED_EDGE ( 'NONE', *, *, #14151, .F. ) ;
#13873 = EDGE_CURVE ( 'NONE', #8986, #9154, #7041, .T. ) ;
#13874 = ORIENTED_EDGE ( 'NONE', *, *, #6993, .T. ) ;
#13875 = CARTESIAN_POINT ( 'NONE',  ( -3.492279824153255330, -5.546088562373062025, 1.060777629467175132 ) ) ;
#13876 = CARTESIAN_POINT ( 'NONE',  ( 2.481497852716095132, -0.7256250000000298295, -3.025965195089417747 ) ) ;
#13877 = ADVANCED_FACE ( 'NONE', ( #9856 ), #13443, .F. ) ;
#13878 = LINE ( 'NONE', #14318, #1876 ) ;
#13879 = CARTESIAN_POINT ( 'NONE',  ( -3.563986660466321510, -2.578124999999990230, 1.906655726273616125 ) ) ;
#13880 = FACE_OUTER_BOUND ( 'NONE', #3167, .T. ) ;
#13881 = CYLINDRICAL_SURFACE ( 'NONE', #9819, 2.500000000000002220 ) ;
#13882 = DIRECTION ( 'NONE',  ( -1.000000000000000000, 0.000000000000000000, 0.000000000000000000 ) ) ;
#13883 = CARTESIAN_POINT ( 'NONE',  ( -86.77438362643999881, 65.17411849586700612, -147.9984795835769944 ) ) ;
#13884 = DIRECTION ( 'NONE',  ( -9.422394424380278809E-16, 1.000000000000000000, -0.000000000000000000 ) ) ;
#13885 = DIRECTION ( 'NONE',  ( -0.000000000000000000, -1.000000000000000000, -0.000000000000000000 ) ) ;
#13886 = EDGE_CURVE ( 'NONE', #12703, #12970, #12271, .T. ) ;
#13887 = ORIENTED_EDGE ( 'NONE', *, *, #14608, .F. ) ;
#13888 = DIRECTION ( 'NONE',  ( 0.000000000000000000, 0.000000000000000000, 1.000000000000000000 ) ) ;
#13889 = VERTEX_POINT ( 'NONE', #13210 ) ;
#13890 = ORIENTED_EDGE ( 'NONE', *, *, #1366, .T. ) ;
#13891 = ORIENTED_EDGE ( 'NONE', *, *, #12541, .F. ) ;
#13892 = EDGE_CURVE ( 'NONE', #6831, #9509, #579, .T. ) ;
#13893 = VECTOR ( 'NONE', #5895, 1000.000000000000000 ) ;
#13894 = DIRECTION ( 'NONE',  ( 1.000000000000000000, 0.000000000000000000, 0.000000000000000000 ) ) ;
#13895 = CARTESIAN_POINT ( 'NONE',  ( -0.3313405146688110925, -4.850625000000119869, -3.351331461923120703 ) ) ;
#13896 = EDGE_CURVE ( 'NONE', #13826, #1753, #10951, .T. ) ;
#13897 = EDGE_CURVE ( 'NONE', #2678, #14347, #480, .T. ) ;
#13898 = CARTESIAN_POINT ( 'NONE',  ( 0.000000000000000000, 0.000000000000000000, 0.000000000000000000 ) ) ;
#13899 = CARTESIAN_POINT ( 'NONE',  ( 2.598076211353315124, 0.1227504548087477720, 4.500000000000000000 ) ) ;
#13900 = CARTESIAN_POINT ( 'NONE',  ( 1.771711357391134500, 2.042612654333142430, -4.500000000000000000 ) ) ;
#13901 = FACE_OUTER_BOUND ( 'NONE', #1760, .T. ) ;
#13902 = VECTOR ( 'NONE', #13558, 1000.000000000000000 ) ;
#13903 = DIRECTION ( 'NONE',  ( -0.4999999999999832356, 0.000000000000000000, -0.8660254037844483666 ) ) ;
#13904 = CARTESIAN_POINT ( 'NONE',  ( -3.884436258901674766, -0.4995676945082689335, 1.749149344944205042 ) ) ;
#13905 = CARTESIAN_POINT ( 'NONE',  ( -50.73238362643999722, 66.35306774555222376, -150.4984795835770228 ) ) ;
#13906 = VECTOR ( 'NONE', #9478, 1000.000000000000114 ) ;
#13907 = ORIENTED_EDGE ( 'NONE', *, *, #4809, .T. ) ;
#13908 = CARTESIAN_POINT ( 'NONE',  ( -3.637955631634631981, -5.500000000000012434, -2.540370839878330420E-14 ) ) ;
#13909 = ORIENTED_EDGE ( 'NONE', *, *, #6508, .F. ) ;
#13910 = VERTEX_POINT ( 'NONE', #14663 ) ;
#13911 = CARTESIAN_POINT ( 'NONE',  ( 0.8000000000000113687, 9.500000000000000000, 9.797174393178965434E-17 ) ) ;
#13912 = ORIENTED_EDGE ( 'NONE', *, *, #346, .F. ) ;
#13913 = CIRCLE ( 'NONE', #2258, 2.577850803773722443 ) ;
#13914 = CARTESIAN_POINT ( 'NONE',  ( -1.221455774822097329, -1.296874999999898082, -4.030457444822014956 ) ) ;
#13915 = ORIENTED_EDGE ( 'NONE', *, *, #13122, .T. ) ;
#13916 = CARTESIAN_POINT ( 'NONE',  ( -0.001440864359646425088, -3.249213562373088227, -3.953673997506742754 ) ) ;
#13917 = AXIS2_PLACEMENT_3D ( 'NONE', #8172, #7248, #7329 ) ;
#13918 = DIRECTION ( 'NONE',  ( -0.9961946980917452121, 3.779777825264100874E-17, -0.08715574274766163532 ) ) ;
#13919 = AXIS2_PLACEMENT_3D ( 'NONE', #4476, #7965, #14021 ) ;
#13920 = LINE ( 'NONE', #2204, #12293 ) ;
#13921 = CARTESIAN_POINT ( 'NONE',  ( -15.50000000000000000, -0.2038245569916614930, -21.05662432702600029 ) ) ;
#13922 = VECTOR ( 'NONE', #11499, 1000.000000000000000 ) ;
#13923 = CARTESIAN_POINT ( 'NONE',  ( -4.486254801108944257, 11.99999970914572778, 69.62284035768031742 ) ) ;
#13924 = LINE ( 'NONE', #9346, #5392 ) ;
#13925 = CARTESIAN_POINT ( 'NONE',  ( 7.511572993685698521E-16, 1.916901515185129432E-30, 4.500000000000000888 ) ) ;
#13926 = AXIS2_PLACEMENT_3D ( 'NONE', #13057, #9460, #14281 ) ;
#13927 = CIRCLE ( 'NONE', #7504, 2.500000000000002220 ) ;
#13928 = DIRECTION ( 'NONE',  ( 0.1143822652403497647, -0.4749580438663243975, 0.8725431530676067693 ) ) ;
#13929 = EDGE_LOOP ( 'NONE', ( #7890, #2352, #4208, #5114 ) ) ;
#13930 = CARTESIAN_POINT ( 'NONE',  ( -2.814361612698371484, -0.2100000000001143730, 2.816411668391418210 ) ) ;
#13931 = VERTEX_POINT ( 'NONE', #7238 ) ;
#13932 = AXIS2_PLACEMENT_3D ( 'NONE', #14940, #4104, #12483 ) ;
#13933 = CARTESIAN_POINT ( 'NONE',  ( 3.503842902704710216, -2.631874999999911147, -1.061889326425361268 ) ) ;
#13934 = DIRECTION ( 'NONE',  ( 0.000000000000000000, 0.000000000000000000, -1.000000000000000000 ) ) ;
#13935 = DIRECTION ( 'NONE',  ( 0.000000000000000000, 0.000000000000000000, -1.000000000000000000 ) ) ;
#13936 = DIRECTION ( 'NONE',  ( -0.000000000000000000, -0.000000000000000000, 1.000000000000000000 ) ) ;
#13937 = CARTESIAN_POINT ( 'NONE',  ( 17.18164641901421419, 11.39999970914576011, 0.8664120436859875651 ) ) ;
#13938 = PLANE ( 'NONE',  #8471 ) ;
#13939 = AXIS2_PLACEMENT_3D ( 'NONE', #7811, #8326, #8400 ) ;
#13940 = ORIENTED_EDGE ( 'NONE', *, *, #6253, .T. ) ;
#13941 = DIRECTION ( 'NONE',  ( 0.000000000000000000, 0.9860132971832695770, 0.1666666666666655749 ) ) ;
#13942 = ADVANCED_FACE ( 'NONE', ( #170 ), #3896, .T. ) ;
#13943 = VERTEX_POINT ( 'NONE', #4917 ) ;
#13944 = EDGE_LOOP ( 'NONE', ( #2700, #709, #591, #7028, #7309, #7408, #468, #14517, #13844, #7899, #15309, #1464, #5189, #685 ) ) ;
#13945 = CARTESIAN_POINT ( 'NONE',  ( 1.614039610742502795, -4.413124999999970655, 3.021508266705728030 ) ) ;
#13946 = ORIENTED_EDGE ( 'NONE', *, *, #345, .T. ) ;
#13947 = ORIENTED_EDGE ( 'NONE', *, *, #7272, .F. ) ;
#13948 = CIRCLE ( 'NONE', #571, 2.500000000000002220 ) ;
#13949 = ORIENTED_EDGE ( 'NONE', *, *, #706, .T. ) ;
#13950 = CARTESIAN_POINT ( 'NONE',  ( 15.50000000000000000, 998.9628421096749662, -22.50000000000000000 ) ) ;
#13951 = CARTESIAN_POINT ( 'NONE',  ( 1.801006600569655891, -1.413124999999811449, 3.371562913404185569 ) ) ;
#13952 = VECTOR ( 'NONE', #10386, 1000.000000000000000 ) ;
#13953 = DIRECTION ( 'NONE',  ( 0.000000000000000000, 0.000000000000000000, 1.000000000000000000 ) ) ;
#13954 = CARTESIAN_POINT ( 'NONE',  ( -2.264039642164870969, -2.343749999999985789, -3.385713959793517080 ) ) ;
#13955 = FACE_OUTER_BOUND ( 'NONE', #2308, .T. ) ;
#13956 = DIRECTION ( 'NONE',  ( 1.000000000000000000, 0.000000000000000000, 0.000000000000000000 ) ) ;
#13957 = CARTESIAN_POINT ( 'NONE',  ( -56.52438362643999170, 65.17411849586700612, -150.4984795835770228 ) ) ;
#13958 = CARTESIAN_POINT ( 'NONE',  ( -37.27438362644000591, 104.6741184958670061, -152.4984795835769944 ) ) ;
#13959 = EDGE_CURVE ( 'NONE', #2626, #11629, #2725, .T. ) ;
#13960 = EDGE_CURVE ( 'NONE', #7132, #11742, #9624, .T. ) ;
#13961 = FACE_OUTER_BOUND ( 'NONE', #5861, .T. ) ;
#13962 = CIRCLE ( 'NONE', #2310, 2.042000000000002036 ) ;
#13963 = CYLINDRICAL_SURFACE ( 'NONE', #14691, 4.500000000000003553 ) ;
#13964 = ORIENTED_EDGE ( 'NONE', *, *, #5675, .F. ) ;
#13965 = CARTESIAN_POINT ( 'NONE',  ( -88.81638362644000040, 63.99516924618178848, -150.4984795835770228 ) ) ;
#13966 = ORIENTED_EDGE ( 'NONE', *, *, #13434, .F. ) ;
#13967 = VERTEX_POINT ( 'NONE', #7474 ) ;
#13968 = ORIENTED_EDGE ( 'NONE', *, *, #8879, .F. ) ;
#13969 = DIRECTION ( 'NONE',  ( 0.9961946980917452121, 0.000000000000000000, 0.08715574274766160756 ) ) ;
#13970 = AXIS2_PLACEMENT_3D ( 'NONE', #9695, #5286, #2793 ) ;
#13971 = CONICAL_SURFACE ( 'NONE', #13739, 3.173335668876520632, 0.9162978572970248425 ) ;
#13972 = EDGE_CURVE ( 'NONE', #8717, #4666, #13244, .T. ) ;
#13973 = FILL_AREA_STYLE ('',( #14284 ) ) ;
#13974 = ADVANCED_FACE ( 'NONE', ( #2654, #1562, #6318 ), #4982, .T. ) ;
#13975 = CARTESIAN_POINT ( 'NONE',  ( 15.50000000000000000, -5.000000000000000000, 26.50000000000000000 ) ) ;
#13976 = DIRECTION ( 'NONE',  ( 0.000000000000000000, -0.000000000000000000, 1.000000000000000000 ) ) ;
#13977 = CARTESIAN_POINT ( 'NONE',  ( -86.27438362644001302, 82.17411849586700612, -150.4984795835769944 ) ) ;
#13978 = CARTESIAN_POINT ( 'NONE',  ( -69.77438362644001302, 110.1741184958670061, -152.4984795835769944 ) ) ;
#13979 = DIRECTION ( 'NONE',  ( 0.000000000000000000, 1.000000000000000000, 0.000000000000000000 ) ) ;
#13980 = DIRECTION ( 'NONE',  ( 0.000000000000000000, 1.000000000000000000, 0.000000000000000000 ) ) ;
#13981 = EDGE_CURVE ( 'NONE', #3702, #14751, #3961, .T. ) ;
#13982 = ORIENTED_EDGE ( 'NONE', *, *, #5958, .T. ) ;
#13983 = DIRECTION ( 'NONE',  ( 0.000000000000000000, 0.000000000000000000, 1.000000000000000000 ) ) ;
#13984 = CIRCLE ( 'NONE', #5830, 0.5999999999999998668 ) ;
#13985 = EDGE_CURVE ( 'NONE', #12733, #4114, #1554, .T. ) ;
#13986 = VERTEX_POINT ( 'NONE', #11100 ) ;
#13987 = EDGE_CURVE ( 'NONE', #10037, #12810, #8535, .T. ) ;
#13988 = ORIENTED_EDGE ( 'NONE', *, *, #6040, .F. ) ;
#13989 = DIRECTION ( 'NONE',  ( -9.422394424380278809E-16, 1.000000000000000000, -0.000000000000000000 ) ) ;
#13990 = EDGE_LOOP ( 'NONE', ( #7993, #6848, #10298, #2040 ) ) ;
#13991 = CARTESIAN_POINT ( 'NONE',  ( 3.738955316585249822, -1.078124999999896527, -2.000248979885406619 ) ) ;
#13992 = ORIENTED_EDGE ( 'NONE', *, *, #7665, .T. ) ;
#13993 = CARTESIAN_POINT ( 'NONE',  ( -3.466325857683220324, -3.421088562373224562, -1.853959688331944244 ) ) ;
#13994 = EDGE_CURVE ( 'NONE', #11184, #3974, #3888, .T. ) ;
#13995 = CARTESIAN_POINT ( 'NONE',  ( -52.77438362643999881, 62.81621999649657084, -147.9984795835769944 ) ) ;
#13996 = DIRECTION ( 'NONE',  ( 0.000000000000000000, 1.000000000000000000, 0.000000000000000000 ) ) ;
#13997 = AXIS2_PLACEMENT_3D ( 'NONE', #12438, #10160, #4365 ) ;
#13998 = CARTESIAN_POINT ( 'NONE',  ( 2.598076211353310239, 1.678847577293378857, -4.499999999999999112 ) ) ;
#13999 = AXIS2_PLACEMENT_3D ( 'NONE', #7776, #7851, #13820 ) ;
#14000 = EDGE_CURVE ( 'NONE', #1058, #14010, #13587, .T. ) ;
#14001 = CARTESIAN_POINT ( 'NONE',  ( -65.90140028023257912, 89.17411849586700612, -57.99847958357699440 ) ) ;
#14002 = ORIENTED_EDGE ( 'NONE', *, *, #6881, .F. ) ;
#14003 = DIRECTION ( 'NONE',  ( -0.000000000000000000, -0.000000000000000000, 1.000000000000000000 ) ) ;
#14004 = DIRECTION ( 'NONE',  ( 0.9999934663667180423, -0.000000000000000000, 0.003614861529253208996 ) ) ;
#14005 = CLOSED_SHELL ( 'NONE', ( #11152, #3717, #6113, #7377, #10568, #10617, #3557, #11819, #4469, #8967, #14139, #2472, #5940, #3570, #7087 ) ) ;
#14006 = ORIENTED_EDGE ( 'NONE', *, *, #12740, .F. ) ;
#14007 = AXIS2_PLACEMENT_3D ( 'NONE', #14240, #11921, #4943 ) ;
#14008 = SURFACE_STYLE_FILL_AREA ( #15079 ) ;
#14009 = CARTESIAN_POINT ( 'NONE',  ( -0.7612222386588008982, -0.8662499999999671019, -3.819631723157197012 ) ) ;
#14010 = VERTEX_POINT ( 'NONE', #2876 ) ;
#14011 = VECTOR ( 'NONE', #1160, 1000.000000000000000 ) ;
#14012 = CARTESIAN_POINT ( 'NONE',  ( -2.013335231365204425, -2.928749999999985310, -3.010762893885847280 ) ) ;
#14013 = DIRECTION ( 'NONE',  ( 0.000000000000000000, 0.000000000000000000, 1.000000000000000000 ) ) ;
#14014 = CIRCLE ( 'NONE', #2628, 1.999999999999988010 ) ;
#14015 = FACE_OUTER_BOUND ( 'NONE', #4959, .T. ) ;
#14016 = CIRCLE ( 'NONE', #4862, 2.500000000000002220 ) ;
#14017 = DIRECTION ( 'NONE',  ( -0.000000000000000000, 1.000000000000000000, -0.000000000000000000 ) ) ;
#14018 = CARTESIAN_POINT ( 'NONE',  ( 15.50000000000000000, 0.000000000000000000, 18.50000000000000000 ) ) ;
#14019 = AXIS2_PLACEMENT_3D ( 'NONE', #7130, #1291, #11849 ) ;
#14020 = DIRECTION ( 'NONE',  ( 0.000000000000000000, 0.000000000000000000, -1.000000000000000000 ) ) ;
#14021 = DIRECTION ( 'NONE',  ( -1.000000000000000000, 0.000000000000000000, 0.000000000000000000 ) ) ;
#14022 = VERTEX_POINT ( 'NONE', #8687 ) ;
#14023 = CARTESIAN_POINT ( 'NONE',  ( -35.58670980944424400, 5.000000000000001776, 125.5408111191910763 ) ) ;
#14024 = ORIENTED_EDGE ( 'NONE', *, *, #521, .T. ) ;
#14025 = VERTEX_POINT ( 'NONE', #6310 ) ;
#14026 = CARTESIAN_POINT ( 'NONE',  ( 3.333123593314366584, -4.616249999999967990, -0.6642911394208930176 ) ) ;
#14027 = EDGE_LOOP ( 'NONE', ( #9665, #4117, #4059 ) ) ;
#14028 = CIRCLE ( 'NONE', #12303, 1.000000000000000888 ) ;
#14029 = EDGE_LOOP ( 'NONE', ( #1500, #13940, #4806, #4302, #13429, #3299 ) ) ;
#14030 = VERTEX_POINT ( 'NONE', #2952 ) ;
#14031 = AXIS2_PLACEMENT_3D ( 'NONE', #10559, #10479, #4680 ) ;
#14032 = CARTESIAN_POINT ( 'NONE',  ( -2.041896248660992175, -5.342963562372913700, -3.057627329919577086 ) ) ;
#14033 = VECTOR ( 'NONE', #8937, 1000.000000000000000 ) ;
#14034 = CARTESIAN_POINT ( 'NONE',  ( 0.3898743713140499501, -0.3506250000000236122, 3.943731105175205975 ) ) ;
#14035 = CARTESIAN_POINT ( 'NONE',  ( -2.598076211353321341, 2.374999999999993339, -4.499999999999999112 ) ) ;
#14036 = DIRECTION ( 'NONE',  ( 1.224646799147351975E-16, 1.000000000000000000, 0.000000000000000000 ) ) ;
#14037 = ADVANCED_FACE ( 'NONE', ( #13362 ), #6233, .T. ) ;
#14038 = DIRECTION ( 'NONE',  ( -2.551930889570659960E-15, 1.000000000000000000, 0.000000000000000000 ) ) ;
#14039 = DIRECTION ( 'NONE',  ( 0.000000000000000000, 1.000000000000000000, 0.000000000000000000 ) ) ;
#14040 = CARTESIAN_POINT ( 'NONE',  ( -69.77438362644001302, 74.17411849586699191, -79.59847958357700293 ) ) ;
#14041 = VECTOR ( 'NONE', #15231, 1000.000000000000000 ) ;
#14042 = LINE ( 'NONE', #9449, #13011 ) ;
#14043 = LINE ( 'NONE', #9149, #889 ) ;
#14044 = CARTESIAN_POINT ( 'NONE',  ( 0.9808155824294413350, -4.788124999999903153, -3.230360883553721862 ) ) ;
#14045 = AXIS2_PLACEMENT_3D ( 'NONE', #7912, #11481, #8850 ) ;
#14046 = ORIENTED_EDGE ( 'NONE', *, *, #11722, .T. ) ;
#14047 = DIRECTION ( 'NONE',  ( 0.000000000000000000, 0.000000000000000000, -1.000000000000000000 ) ) ;
#14048 = ORIENTED_EDGE ( 'NONE', *, *, #9491, .F. ) ;
#14049 = VERTEX_POINT ( 'NONE', #5138 ) ;
#14050 = VERTEX_POINT ( 'NONE', #14652 ) ;
#14051 =( NAMED_UNIT ( * ) PLANE_ANGLE_UNIT ( ) SI_UNIT ( $, .RADIAN. ) );
#14052 = VECTOR ( 'NONE', #15212, 1000.000000000000000 ) ;
#14053 = EDGE_CURVE ( 'NONE', #7246, #1528, #10254, .T. ) ;
#14054 = CARTESIAN_POINT ( 'NONE',  ( 0.6569748927284305706, -4.803749999999888054, -3.309289439050846937 ) ) ;
#14055 = CIRCLE ( 'NONE', #11575, 1.199999999999999734 ) ;
#14056 = LINE ( 'NONE', #15122, #14280 ) ;
#14057 = CARTESIAN_POINT ( 'NONE',  ( 21.98164641901421135, -12.00000029085423670, -14.13358795631400611 ) ) ;
#14058 = DIRECTION ( 'NONE',  ( 1.000000000000000000, 0.000000000000000000, 0.000000000000000000 ) ) ;
#14059 = EDGE_CURVE ( 'NONE', #12175, #3871, #12180, .T. ) ;
#14060 = PLANE ( 'NONE',  #4132 ) ;
#14061 = CARTESIAN_POINT ( 'NONE',  ( -91.02438362643999881, 65.17411849586700612, -145.4984795835769660 ) ) ;
#14062 = LINE ( 'NONE', #2421, #78 ) ;
#14063 = LINE ( 'NONE', #11, #1363 ) ;
#14064 = PLANE ( 'NONE',  #12973 ) ;
#14065 = EDGE_LOOP ( 'NONE', ( #1438, #4278, #3037, #12788 ) ) ;
#14066 = CARTESIAN_POINT ( 'NONE',  ( 22.58164641901421632, -2.908542394189813650E-07, -0.3335879563140091153 ) ) ;
#14067 = ORIENTED_EDGE ( 'NONE', *, *, #11382, .F. ) ;
#14068 = CIRCLE ( 'NONE', #3661, 5.500000000000005329 ) ;
#14069 = ORIENTED_EDGE ( 'NONE', *, *, #1746, .T. ) ;
#14070 = DIRECTION ( 'NONE',  ( 1.000000000000000000, 0.000000000000000000, 0.000000000000000000 ) ) ;
#14071 = VERTEX_POINT ( 'NONE', #10942 ) ;
#14072 = CARTESIAN_POINT ( 'NONE',  ( 2.992932217727461097, -1.124999999999971800, -2.995094308971279151 ) ) ;
#14073 = ORIENTED_EDGE ( 'NONE', *, *, #3751, .F. ) ;
#14074 = EDGE_CURVE ( 'NONE', #13685, #8016, #10004, .T. ) ;
#14075 = CARTESIAN_POINT ( 'NONE',  ( 4.097285757785106952, -2.014838562373181485, -0.4024520375138228578 ) ) ;
#14076 = DIRECTION ( 'NONE',  ( 0.000000000000000000, 1.000000000000000000, 0.000000000000000000 ) ) ;
#14077 = ADVANCED_FACE ( 'NONE', ( #13509 ), #4323, .F. ) ;
#14078 = FACE_BOUND ( 'NONE', #2001, .T. ) ;
#14079 = AXIS2_PLACEMENT_3D ( 'NONE', #13367, #1561, #6317 ) ;
#14080 = ADVANCED_FACE ( 'NONE', ( #13283 ), #12264, .T. ) ;
#14081 = DIRECTION ( 'NONE',  ( 0.000000000000000000, 0.000000000000000000, -1.000000000000000000 ) ) ;
#14082 = CARTESIAN_POINT ( 'NONE',  ( 17.23697745638123280, -3.654316742536412033, -0.03314156585704672309 ) ) ;
#14083 = ORIENTED_EDGE ( 'NONE', *, *, #40, .T. ) ;
#14084 = LINE ( 'NONE', #7116, #12314 ) ;
#14085 = FACE_OUTER_BOUND ( 'NONE', #6551, .T. ) ;
#14086 = EDGE_CURVE ( 'NONE', #2967, #2765, #1707, .T. ) ;
#14087 = ORIENTED_EDGE ( 'NONE', *, *, #14369, .T. ) ;
#14088 = AXIS2_PLACEMENT_3D ( 'NONE', #1619, #9753, #1472 ) ;
#14089 = LINE ( 'NONE', #12925, #3603 ) ;
#14090 = CARTESIAN_POINT ( 'NONE',  ( 0.3898743713140983003, -0.3506250000000236122, 3.943731105175303231 ) ) ;
#14091 = VERTEX_POINT ( 'NONE', #4119 ) ;
#14092 = EDGE_CURVE ( 'NONE', #10812, #12871, #13489, .T. ) ;
#14093 = CARTESIAN_POINT ( 'NONE',  ( -2.629016928070645243, -2.210000000000078568, 2.627652665972809665 ) ) ;
#14094 = EDGE_CURVE ( 'NONE', #9286, #4436, #3807, .T. ) ;
#14095 = EDGE_CURVE ( 'NONE', #11599, #7739, #7392, .T. ) ;
#14096 = DIRECTION ( 'NONE',  ( 1.000000000000000000, 0.000000000000000000, 0.000000000000000000 ) ) ;
#14097 = CARTESIAN_POINT ( 'NONE',  ( 6.205964732515537312E-15, 4.927357795815634489, 0.000000000000000000 ) ) ;
#14098 = PLANE ( 'NONE',  #5682 ) ;
#14099 = CARTESIAN_POINT ( 'NONE',  ( -80.52077156573417938, 0.000000000000000000, -152.4984795835769944 ) ) ;
#14100 = DIRECTION ( 'NONE',  ( 1.445602896647339163E-16, -1.000000000000000000, 0.000000000000000000 ) ) ;
#14101 = VERTEX_POINT ( 'NONE', #8990 ) ;
#14102 = DIRECTION ( 'NONE',  ( 0.000000000000000000, 0.000000000000000000, -1.000000000000000000 ) ) ;
#14103 = VERTEX_POINT ( 'NONE', #6615 ) ;
#14104 = ORIENTED_EDGE ( 'NONE', *, *, #9680, .F. ) ;
#14105 = EDGE_LOOP ( 'NONE', ( #3493, #11548, #3040, #11697 ) ) ;
#14106 = ORIENTED_EDGE ( 'NONE', *, *, #15269, .F. ) ;
#14107 = ORIENTED_EDGE ( 'NONE', *, *, #9772, .F. ) ;
#14108 = CARTESIAN_POINT ( 'NONE',  ( -1.068188678435922245, -5.296088562372957220, -3.524632553026846082 ) ) ;
#14109 = PLANE ( 'NONE',  #9756 ) ;
#14110 = PLANE ( 'NONE',  #2914 ) ;
#14111 = LINE ( 'NONE', #3481, #3788 ) ;
#14112 = CARTESIAN_POINT ( 'NONE',  ( -69.77438362644100778, 82.17411849586699191, -67.49847958357700861 ) ) ;
#14113 = LINE ( 'NONE', #12960, #460 ) ;
#14114 = DIRECTION ( 'NONE',  ( 0.000000000000000000, 0.000000000000000000, -1.000000000000000000 ) ) ;
#14115 = CARTESIAN_POINT ( 'NONE',  ( 1.581646419014216542, -11.40000029085424238, 0.2664120436859911956 ) ) ;
#14116 = CARTESIAN_POINT ( 'NONE',  ( -35.58670980944424400, 5.000000000000001776, 97.50956111919106206 ) ) ;
#14117 = CARTESIAN_POINT ( 'NONE',  ( 1.592243150387700146, -4.756875000000070131, -2.981552405995577359 ) ) ;
#14118 = LINE ( 'NONE', #14190, #2561 ) ;
#14119 = ORIENTED_EDGE ( 'NONE', *, *, #10446, .T. ) ;
#14120 = LINE ( 'NONE', #11569, #9482 ) ;
#14121 = ORIENTED_EDGE ( 'NONE', *, *, #14733, .T. ) ;
#14122 = VERTEX_POINT ( 'NONE', #12713 ) ;
#14123 = EDGE_LOOP ( 'NONE', ( #7213, #12196, #10469, #8370, #6001 ) ) ;
#14124 = CARTESIAN_POINT ( 'NONE',  ( -2.533829858540697977, -3.209999999999945786, 2.535703909530142575 ) ) ;
#14125 = DIRECTION ( 'NONE',  ( -1.000000000000000000, 0.000000000000000000, 0.000000000000000000 ) ) ;
#14126 = CARTESIAN_POINT ( 'NONE',  ( 66.41329019055577021, 5.000000000000000000, 89.50956111919107627 ) ) ;
#14127 = CARTESIAN_POINT ( 'NONE',  ( -77.52077156573416516, 103.6741184958669777, -79.59847958357700293 ) ) ;
#14128 = CARTESIAN_POINT ( 'NONE',  ( 15.50000000000000000, -2.500000000000000000, 23.94337567297399971 ) ) ;
#14129 = FACE_OUTER_BOUND ( 'NONE', #13553, .T. ) ;
#14130 = CARTESIAN_POINT ( 'NONE',  ( -62.27438362644000591, 90.17411849586700612, -58.99847958357700151 ) ) ;
#14131 = DIRECTION ( 'NONE',  ( 0.000000000000000000, 0.000000000000000000, -1.000000000000000000 ) ) ;
#14132 = LINE ( 'NONE', #7011, #5289 ) ;
#14133 = EDGE_LOOP ( 'NONE', ( #13603, #774 ) ) ;
#14134 = CARTESIAN_POINT ( 'NONE',  ( -59.02799568714584666, 60.67411849586701322, -152.4984795835769944 ) ) ;
#14135 = EDGE_CURVE ( 'NONE', #3706, #8660, #11555, .T. ) ;
#14136 = EDGE_LOOP ( 'NONE', ( #9895, #12654, #2227, #14606 ) ) ;
#14137 = ORIENTED_EDGE ( 'NONE', *, *, #6044, .F. ) ;
#14138 = DIRECTION ( 'NONE',  ( -6.860497997771531562E-15, -6.464231808267455010E-30, -1.000000000000000000 ) ) ;
#14139 = ADVANCED_FACE ( 'NONE', ( #7840 ), #10499, .F. ) ;
#14140 = CARTESIAN_POINT ( 'NONE',  ( 4.382995262527464853, 1.326351951446563815E-13, -0.001575499653098922336 ) ) ;
#14141 = ORIENTED_EDGE ( 'NONE', *, *, #339, .T. ) ;
#14142 = CARTESIAN_POINT ( 'NONE',  ( 3.934944799906381796, -0.9367135623731039917, 1.631135842912540879 ) ) ;
#14143 = VECTOR ( 'NONE', #732, 1000.000000000000000 ) ;
#14144 = DIRECTION ( 'NONE',  ( -0.4999999999999998890, 0.8660254037844387076, 0.000000000000000000 ) ) ;
#14145 = DIRECTION ( 'NONE',  ( -0.8660254037844381525, 0.000000000000000000, -0.5000000000000007772 ) ) ;
#14146 = VECTOR ( 'NONE', #3059, 1000.000000000000114 ) ;
#14147 = CARTESIAN_POINT ( 'NONE',  ( 3.452158817763105070, 2.307268873417427368, -3.020685531837379312 ) ) ;
#14148 = DIRECTION ( 'NONE',  ( 0.000000000000000000, 0.000000000000000000, 1.000000000000000000 ) ) ;
#14149 = EDGE_LOOP ( 'NONE', ( #15230, #3745, #7308, #9903, #13374, #7182 ) ) ;
#14150 = CARTESIAN_POINT ( 'NONE',  ( -3.173335668876506865, -5.500000000000010658, 0.000000000000000000 ) ) ;
#14151 = EDGE_CURVE ( 'NONE', #2748, #682, #5680, .T. ) ;
#14152 = CARTESIAN_POINT ( 'NONE',  ( -75.01311196519617397, 67.29799558322736175, -83.44847958357698303 ) ) ;
#14153 = AXIS2_PLACEMENT_3D ( 'NONE', #8253, #8412, #11829 ) ;
#14154 = ORIENTED_EDGE ( 'NONE', *, *, #1553, .F. ) ;
#14155 = ADVANCED_FACE ( 'NONE', ( #14872 ), #7231, .T. ) ;
#14156 = CIRCLE ( 'NONE', #5749, 3.499999999999999556 ) ;
#14157 = CARTESIAN_POINT ( 'NONE',  ( -1.491583768208377681, -3.687499999999984901, 3.598334897712680114 ) ) ;
#14158 = ORIENTED_EDGE ( 'NONE', *, *, #9675, .T. ) ;
#14159 = AXIS2_PLACEMENT_3D ( 'NONE', #1699, #7829, #7757 ) ;
#14160 = CARTESIAN_POINT ( 'NONE',  ( -2.381388125886219509, -1.944375000000168052, -2.899558211763606064 ) ) ;
#14161 = AXIS2_PLACEMENT_3D ( 'NONE', #12370, #14527, #6336 ) ;
#14162 = EDGE_CURVE ( 'NONE', #1380, #13125, #12252, .T. ) ;
#14163 = EDGE_CURVE ( 'NONE', #1856, #8800, #5817, .T. ) ;
#14164 = FACE_OUTER_BOUND ( 'NONE', #14029, .T. ) ;
#14165 = FACE_BOUND ( 'NONE', #13672, .T. ) ;
#14166 = VECTOR ( 'NONE', #2515, 1000.000000000000114 ) ;
#14167 = ADVANCED_FACE ( 'NONE', ( #3558 ), #6065, .F. ) ;
#14168 = DIRECTION ( 'NONE',  ( 0.000000000000000000, 1.000000000000000000, 0.000000000000000000 ) ) ;
#14169 = VERTEX_POINT ( 'NONE', #139 ) ;
#14170 = FACE_OUTER_BOUND ( 'NONE', #6142, .T. ) ;
#14171 = ORIENTED_EDGE ( 'NONE', *, *, #10146, .T. ) ;
#14172 = ADVANCED_FACE ( 'NONE', ( #1304 ), #8141, .T. ) ;
#14173 = AXIS2_PLACEMENT_3D ( 'NONE', #679, #4182, #13720 ) ;
#14174 = DIRECTION ( 'NONE',  ( 0.000000000000000000, 1.000000000000000000, 0.000000000000000000 ) ) ;
#14175 = EDGE_CURVE ( 'NONE', #1550, #4558, #8772, .T. ) ;
#14176 = ORIENTED_EDGE ( 'NONE', *, *, #1553, .T. ) ;
#14177 = ORIENTED_EDGE ( 'NONE', *, *, #13048, .T. ) ;
#14178 = ORIENTED_EDGE ( 'NONE', *, *, #1933, .T. ) ;
#14179 = CARTESIAN_POINT ( 'NONE',  ( 3.272906902298228005, -5.077338562373189923, -1.750952971977949968 ) ) ;
#14180 = VECTOR ( 'NONE', #3270, 1000.000000000000000 ) ;
#14181 = DIRECTION ( 'NONE',  ( 1.000000000000000000, 1.727704675731647582E-15, 0.000000000000000000 ) ) ;
#14182 = CYLINDRICAL_SURFACE ( 'NONE', #6380, 8.124999999999992895 ) ;
#14183 = DIRECTION ( 'NONE',  ( -1.000000000000000000, 0.000000000000000000, 0.000000000000000000 ) ) ;
#14184 = CARTESIAN_POINT ( 'NONE',  ( -86.77438362644001302, 65.17411849586700612, -152.4984795835769944 ) ) ;
#14185 = AXIS2_PLACEMENT_3D ( 'NONE', #14243, #12086, #3776 ) ;
#14186 = CARTESIAN_POINT ( 'NONE',  ( -23.25000000000000000, 0.000000000000000000, -27.00000000000000000 ) ) ;
#14187 = FACE_OUTER_BOUND ( 'NONE', #11060, .T. ) ;
#14188 = EDGE_CURVE ( 'NONE', #14573, #10111, #1341, .T. ) ;
#14189 = CARTESIAN_POINT ( 'NONE',  ( 2.928286698324767290, -3.678750000000110987, -1.958188979435658839 ) ) ;
#14190 = CARTESIAN_POINT ( 'NONE',  ( -66.41143315690761995, 66.60412428008086749, -81.84847958357698872 ) ) ;
#14191 = ORIENTED_EDGE ( 'NONE', *, *, #8027, .T. ) ;
#14192 = CARTESIAN_POINT ( 'NONE',  ( -86.77438362643999881, 65.17411849586700612, -79.59847958357700293 ) ) ;
#14193 = VECTOR ( 'NONE', #6621, 1000.000000000000000 ) ;
#14194 = CIRCLE ( 'NONE', #7527, 2.500000000000002220 ) ;
#14195 = ORIENTED_EDGE ( 'NONE', *, *, #6128, .F. ) ;
#14196 = EDGE_LOOP ( 'NONE', ( #11167, #4226, #3441, #7903 ) ) ;
#14197 = ORIENTED_EDGE ( 'NONE', *, *, #1570, .F. ) ;
#14198 = CIRCLE ( 'NONE', #7530, 1.250000000000001110 ) ;
#14199 = CARTESIAN_POINT ( 'NONE',  ( 22.28931995216796835, 10.99999970914572778, 69.13384072020835447 ) ) ;
#14200 = CARTESIAN_POINT ( 'NONE',  ( -1.707523105661799434, -2.913124999999936904, -3.196535590052164810 ) ) ;
#14201 = DIRECTION ( 'NONE',  ( -0.4999999999999998890, 0.8660254037844387076, 0.000000000000000000 ) ) ;
#14202 = FACE_OUTER_BOUND ( 'NONE', #6423, .T. ) ;
#14203 = CONICAL_SURFACE ( 'NONE', #7030, 3.968749999999992895, 0.7155849933176756661 ) ;
#14204 = DIRECTION ( 'NONE',  ( 0.000000000000000000, -0.000000000000000000, -1.000000000000000000 ) ) ;
#14205 = CIRCLE ( 'NONE', #2069, 10.50000000000000178 ) ;
#14206 = DIRECTION ( 'NONE',  ( 1.000000000000000000, 0.000000000000000000, -1.284980352575412699E-16 ) ) ;
#14207 = DIRECTION ( 'NONE',  ( -1.000000000000000000, 0.000000000000000000, 0.000000000000000000 ) ) ;
#14208 = FACE_OUTER_BOUND ( 'NONE', #8929, .T. ) ;
#14209 = DIRECTION ( 'NONE',  ( -1.000000000000000000, 0.000000000000000000, 0.000000000000000000 ) ) ;
#14210 = LINE ( 'NONE', #14293, #6119 ) ;
#14211 = LINE ( 'NONE', #9548, #566 ) ;
#14212 = AXIS2_PLACEMENT_3D ( 'NONE', #28, #3524, #8345 ) ;
#14213 = ORIENTED_EDGE ( 'NONE', *, *, #11682, .T. ) ;
#14214 = CARTESIAN_POINT ( 'NONE',  ( -15.50000000000000000, -5.000000000000000000, -19.00000000000000000 ) ) ;
#14215 = EDGE_LOOP ( 'NONE', ( #1549, #11299, #2786, #9137 ) ) ;
#14216 = EDGE_LOOP ( 'NONE', ( #8384, #260, #11723, #8228 ) ) ;
#14217 = CARTESIAN_POINT ( 'NONE',  ( -16.75000000000000000, -0.2714405302574915413, -22.01253933645463334 ) ) ;
#14218 = AXIS2_PLACEMENT_3D ( 'NONE', #12212, #1586, #6339 ) ;
#14219 = VECTOR ( 'NONE', #3876, 1000.000000000000000 ) ;
#14220 = EDGE_LOOP ( 'NONE', ( #5438, #9198, #12036, #12972 ) ) ;
#14221 = CARTESIAN_POINT ( 'NONE',  ( 4.165833326811591242, -1.030463562373184150, -0.8274826639205559164 ) ) ;
#14222 = DIRECTION ( 'NONE',  ( 0.000000000000000000, 0.000000000000000000, -1.000000000000000000 ) ) ;
#14223 = CARTESIAN_POINT ( 'NONE',  ( 0.000000000000000000, -5.000000000000000000, 0.000000000000000000 ) ) ;
#14224 = CARTESIAN_POINT ( 'NONE',  ( 2.802265715718417205, 1.883037081658679446, -4.146333404067327422 ) ) ;
#14225 = CIRCLE ( 'NONE', #1845, 0.6000000000000000888 ) ;
#14226 = EDGE_CURVE ( 'NONE', #11654, #557, #9520, .T. ) ;
#14227 = AXIS2_PLACEMENT_3D ( 'NONE', #1288, #8426, #12084 ) ;
#14228 = FACE_OUTER_BOUND ( 'NONE', #7291, .T. ) ;
#14229 = ORIENTED_EDGE ( 'NONE', *, *, #10080, .F. ) ;
#14230 = CARTESIAN_POINT ( 'NONE',  ( 3.519594483087749914, -5.184756082317176329, -0.7836709140574362742 ) ) ;
#14231 = DIRECTION ( 'NONE',  ( 1.000000000000000000, 0.000000000000000000, 0.000000000000000000 ) ) ;
#14232 = SHAPE_DEFINITION_REPRESENTATION ( #4883, #4448 ) ;
#14233 = ORIENTED_EDGE ( 'NONE', *, *, #3459, .T. ) ;
#14234 = CARTESIAN_POINT ( 'NONE',  ( -3.618276846414829162, -4.546874999999968914, 1.099041561241040466 ) ) ;
#14235 = EDGE_LOOP ( 'NONE', ( #3061, #14889, #8720 ) ) ;
#14236 = VECTOR ( 'NONE', #12882, 1000.000000000000000 ) ;
#14237 = CARTESIAN_POINT ( 'NONE',  ( 3.779448512589415721, -1.600625000000089226, -0.3712484392070565797 ) ) ;
#14238 = FACE_OUTER_BOUND ( 'NONE', #4010, .T. ) ;
#14239 = ADVANCED_FACE ( 'NONE', ( #9597 ), #6980, .F. ) ;
#14240 = CARTESIAN_POINT ( 'NONE',  ( -69.77438362644001302, 82.17411849586700612, -85.04847958357699156 ) ) ;
#14241 = FACE_OUTER_BOUND ( 'NONE', #5051, .T. ) ;
#14242 = LINE ( 'NONE', #1289, #11114 ) ;
#14243 = CARTESIAN_POINT ( 'NONE',  ( -86.77438362644001302, 99.17411849586700612, -86.49847958357699440 ) ) ;
#14244 = DIRECTION ( 'NONE',  ( -1.000000000000000000, -2.459952698498907323E-15, 0.000000000000000000 ) ) ;
#14245 = STYLED_ITEM ( 'NONE', ( #2287 ), #298 ) ;
#14246 = CIRCLE ( 'NONE', #7584, 8.349999999999996092 ) ;
#14247 = ORIENTED_EDGE ( 'NONE', *, *, #7568, .F. ) ;
#14248 = AXIS2_PLACEMENT_3D ( 'NONE', #5833, #8148, #12803 ) ;
#14249 = CARTESIAN_POINT ( 'NONE',  ( 21.98164641901421135, 11.99999970914575798, -0.3335879563140091153 ) ) ;
#14250 = SHAPE_REPRESENTATION_RELATIONSHIP ( 'NONE' , 'NONE' ,  #2929, #3867 ) ;
#14251 = ORIENTED_EDGE ( 'NONE', *, *, #22, .F. ) ;
#14252 = EDGE_CURVE ( 'NONE', #5814, #8210, #14469, .T. ) ;
#14253 = CARTESIAN_POINT ( 'NONE',  ( 15.50000000000000000, -0.4000000000000000222, -19.00000000000000355 ) ) ;
#14254 = CARTESIAN_POINT ( 'NONE',  ( 2.255458548909141214, -3.444374999999939568, 2.746210667320787557 ) ) ;
#14255 = ORIENTED_EDGE ( 'NONE', *, *, #1398, .T. ) ;
#14256 = ORIENTED_EDGE ( 'NONE', *, *, #15102, .T. ) ;
#14257 = ORIENTED_EDGE ( 'NONE', *, *, #8677, .T. ) ;
#14258 = CIRCLE ( 'NONE', #5362, 1.500000000000001332 ) ;
#14259 = CARTESIAN_POINT ( 'NONE',  ( 68.41329019055577021, 5.000000000000000000, 135.5095611191910621 ) ) ;
#14260 = EDGE_CURVE ( 'NONE', #6866, #2365, #5319, .T. ) ;
#14261 = CIRCLE ( 'NONE', #1886, 16.50000000000000000 ) ;
#14262 = AXIS2_PLACEMENT_3D ( 'NONE', #2998, #13632, #13778 ) ;
#14263 = CARTESIAN_POINT ( 'NONE',  ( -4.522482571421200248, -11.00000029085428110, 70.03692566716176771 ) ) ;
#14264 = FACE_OUTER_BOUND ( 'NONE', #7871, .T. ) ;
#14265 = EDGE_CURVE ( 'NONE', #13838, #9398, #6149, .T. ) ;
#14266 = EDGE_CURVE ( 'NONE', #1111, #188, #11784, .T. ) ;
#14267 = CARTESIAN_POINT ( 'NONE',  ( -86.77438362644001302, 65.17411849586700612, -86.49847958357699440 ) ) ;
#14268 = PLANE ( 'NONE',  #9963 ) ;
#14269 = FACE_OUTER_BOUND ( 'NONE', #12308, .T. ) ;
#14270 = CARTESIAN_POINT ( 'NONE',  ( 2.488663048653545928, -3.709999999999854303, -2.487386788893799494 ) ) ;
#14271 = CARTESIAN_POINT ( 'NONE',  ( 0.000000000000000000, 0.000000000000000000, 0.000000000000000000 ) ) ;
#14272 = ORIENTED_EDGE ( 'NONE', *, *, #2519, .F. ) ;
#14273 = DIRECTION ( 'NONE',  ( 0.000000000000000000, 0.000000000000000000, 1.000000000000000000 ) ) ;
#14274 = AXIS2_PLACEMENT_3D ( 'NONE', #14389, #9969, #1372 ) ;
#14275 = ORIENTED_EDGE ( 'NONE', *, *, #8062, .F. ) ;
#14276 = CIRCLE ( 'NONE', #3129, 2.500000000000002220 ) ;
#14277 = ADVANCED_FACE ( 'NONE', ( #11704 ), #8374, .F. ) ;
#14278 = ORIENTED_EDGE ( 'NONE', *, *, #6526, .F. ) ;
#14279 = VERTEX_POINT ( 'NONE', #10532 ) ;
#14280 = VECTOR ( 'NONE', #10555, 1000.000000000000000 ) ;
#14281 = DIRECTION ( 'NONE',  ( 0.000000000000000000, 0.000000000000000000, 1.000000000000000000 ) ) ;
#14282 = CARTESIAN_POINT ( 'NONE',  ( 1.055499318045234114, -2.788125000000055476, -3.484140247641438926 ) ) ;
#14283 = EDGE_CURVE ( 'NONE', #8154, #2658, #11253, .T. ) ;
#14284 = FILL_AREA_STYLE_COLOUR ( '', #6133 ) ;
#14285 = AXIS2_PLACEMENT_3D ( 'NONE', #4296, #6564, #9021 ) ;
#14286 = CARTESIAN_POINT ( 'NONE',  ( -88.81638362644000040, 63.99516924618178848, -147.9984795835769944 ) ) ;
#14287 = DIRECTION ( 'NONE',  ( 0.000000000000000000, 4.336808689942017736E-16, -1.000000000000000000 ) ) ;
#14288 = DIRECTION ( 'NONE',  ( 0.8660254037844482555, 0.000000000000000000, -0.4999999999999831801 ) ) ;
#14289 = CIRCLE ( 'NONE', #168, 1.999999999999986233 ) ;
#14290 = CARTESIAN_POINT ( 'NONE',  ( 2.320576762250993852, 9.355654565435175485, 0.000000000000000000 ) ) ;
#14291 = CARTESIAN_POINT ( 'NONE',  ( -80.52077156573417938, 59.67411849586701322, -152.4984795835769944 ) ) ;
#14292 = DIRECTION ( 'NONE',  ( 0.000000000000000000, -1.000000000000000000, 0.000000000000000000 ) ) ;
#14293 = CARTESIAN_POINT ( 'NONE',  ( 22.58164641901421632, 5.075009326258863140, -11.09921666827752951 ) ) ;
#14294 = DIRECTION ( 'NONE',  ( 0.000000000000000000, 0.000000000000000000, 1.000000000000000000 ) ) ;
#14295 = ORIENTED_EDGE ( 'NONE', *, *, #11325, .F. ) ;
#14296 = PLANE ( 'NONE',  #1315 ) ;
#14297 = ORIENTED_EDGE ( 'NONE', *, *, #8409, .F. ) ;
#14298 = EDGE_LOOP ( 'NONE', ( #15195, #13508, #772, #6646 ) ) ;
#14299 = AXIS2_PLACEMENT_3D ( 'NONE', #14364, #2659, #6179 ) ;
#14300 = AXIS2_PLACEMENT_3D ( 'NONE', #1920, #8902, #11537 ) ;
#14301 = CARTESIAN_POINT ( 'NONE',  ( -1.284862778419491258, 0.2968750000000271450, 4.231539792689364532 ) ) ;
#14302 = ORIENTED_EDGE ( 'NONE', *, *, #1194, .F. ) ;
#14303 = CARTESIAN_POINT ( 'NONE',  ( -4.109106552884008501, -1.467963562373030717, -0.8158076774038809376 ) ) ;
#14304 = CARTESIAN_POINT ( 'NONE',  ( -69.77438362644001302, 82.17411849586700612, -150.4984795835769944 ) ) ;
#14305 = CARTESIAN_POINT ( 'NONE',  ( -52.77438362643999881, 65.17411849586700612, -150.4984795835770228 ) ) ;
#14306 = CARTESIAN_POINT ( 'NONE',  ( -13.41835358098578723, -12.60000029085423812, -8.183940086454239093 ) ) ;
#14307 = CIRCLE ( 'NONE', #6169, 10.50000000000000178 ) ;
#14308 = PLANE ( 'NONE',  #10748 ) ;
#14309 = EDGE_LOOP ( 'NONE', ( #6844, #11661, #3826, #8661 ) ) ;
#14310 = DIRECTION ( 'NONE',  ( 1.000000000000000000, 2.551930889570660354E-15, 0.000000000000000000 ) ) ;
#14311 = CARTESIAN_POINT ( 'NONE',  ( 17.00399103715874460, 11.48932363952878788, 0.2918479299858876552 ) ) ;
#14312 = ORIENTED_EDGE ( 'NONE', *, *, #2044, .T. ) ;
#14313 = LINE ( 'NONE', #3692, #14510 ) ;
#14314 = CARTESIAN_POINT ( 'NONE',  ( -3.331846864947428877, -4.578125000000028422, 1.779793940175935729 ) ) ;
#14315 = ORIENTED_EDGE ( 'NONE', *, *, #4419, .T. ) ;
#14316 = EDGE_CURVE ( 'NONE', #11145, #3516, #7054, .T. ) ;
#14317 = CARTESIAN_POINT ( 'NONE',  ( 0.7459506331255062461, -1.366249999999944897, 3.755271276440939054 ) ) ;
#14318 = CARTESIAN_POINT ( 'NONE',  ( -35.27438362644000591, 59.67411849586700612, -79.49847958357700861 ) ) ;
#14319 = CARTESIAN_POINT ( 'NONE',  ( 57.41329019055577021, 5.000000000000001776, 97.50956111919106206 ) ) ;
#14320 = CARTESIAN_POINT ( 'NONE',  ( -37.27438362644000591, 65.17411849586700612, -15.85886927678779834 ) ) ;
#14321 = DIRECTION ( 'NONE',  ( 0.000000000000000000, 0.000000000000000000, -1.000000000000000000 ) ) ;
#14322 = CARTESIAN_POINT ( 'NONE',  ( -101.2743836264399988, 57.67411849586699901, -67.49847958357700861 ) ) ;
#14323 = DIRECTION ( 'NONE',  ( -0.000000000000000000, 0.000000000000000000, 1.000000000000000000 ) ) ;
#14324 = ORIENTED_EDGE ( 'NONE', *, *, #10470, .T. ) ;
#14325 = CARTESIAN_POINT ( 'NONE',  ( -63.06767964790545022, 68.65632084656354550, -83.44847958357698303 ) ) ;
#14326 = ADVANCED_FACE ( 'NONE', ( #15259 ), #14109, .T. ) ;
#14327 =( NAMED_UNIT ( * ) SI_UNIT ( $, .STERADIAN. ) SOLID_ANGLE_UNIT ( ) );
#14328 = VERTEX_POINT ( 'NONE', #12402 ) ;
#14329 = CARTESIAN_POINT ( 'NONE',  ( -12.81835358098578759, -11.40000029085423705, -11.73358795631401463 ) ) ;
#14330 = CARTESIAN_POINT ( 'NONE',  ( -3.166267757014364914, -3.163124999999988862, 1.693910156975117154 ) ) ;
#14331 = VERTEX_POINT ( 'NONE', #7603 ) ;
#14332 = VERTEX_POINT ( 'NONE', #284 ) ;
#14333 = EDGE_CURVE ( 'NONE', #7802, #632, #9023, .T. ) ;
#14334 = ORIENTED_EDGE ( 'NONE', *, *, #6285, .F. ) ;
#14335 = AXIS2_PLACEMENT_3D ( 'NONE', #358, #8731, #12229 ) ;
#14336 = FACE_OUTER_BOUND ( 'NONE', #11718, .T. ) ;
#14337 = CARTESIAN_POINT ( 'NONE',  ( 15.50000000000000000, 0.000000000000000000, -26.50000000000000000 ) ) ;
#14338 = FACE_OUTER_BOUND ( 'NONE', #2698, .T. ) ;
#14339 = LINE ( 'NONE', #2401, #9047 ) ;
#14340 = CARTESIAN_POINT ( 'NONE',  ( -1.990045403832418236, -3.241250000000046594, 2.976654046991286329 ) ) ;
#14341 = CARTESIAN_POINT ( 'NONE',  ( -54.81638362644000040, 63.99516924618178848, -150.4984795835770228 ) ) ;
#14342 = ORIENTED_EDGE ( 'NONE', *, *, #5287, .F. ) ;
#14343 = DIRECTION ( 'NONE',  ( -0.8660254037844387076, -0.4999999999999998890, 0.000000000000000000 ) ) ;
#14344 = EDGE_CURVE ( 'NONE', #2214, #8981, #1693, .T. ) ;
#14345 = ORIENTED_EDGE ( 'NONE', *, *, #5394, .T. ) ;
#14346 = ORIENTED_EDGE ( 'NONE', *, *, #14659, .T. ) ;
#14347 = VERTEX_POINT ( 'NONE', #9904 ) ;
#14348 = ORIENTED_EDGE ( 'NONE', *, *, #5854, .T. ) ;
#14349 = EDGE_CURVE ( 'NONE', #389, #4822, #13345, .T. ) ;
#14350 = CARTESIAN_POINT ( 'NONE',  ( 23.77513017582411692, -1.718469852516944459E-15, 56.45152858669899132 ) ) ;
#14351 = CARTESIAN_POINT ( 'NONE',  ( 3.376561219002149450, -3.631875000000035048, -1.025635141340205836 ) ) ;
#14352 = CARTESIAN_POINT ( 'NONE',  ( 30.00000000000000000, -5.000000000000000000, -27.00000000000000000 ) ) ;
#14353 = DIRECTION ( 'NONE',  ( 0.000000000000000000, 0.000000000000000000, -1.000000000000000000 ) ) ;
#14354 = CYLINDRICAL_SURFACE ( 'NONE', #6038, 3.000000000000002665 ) ;
#14355 = FACE_OUTER_BOUND ( 'NONE', #14457, .T. ) ;
#14356 = CARTESIAN_POINT ( 'NONE',  ( -16.75000000000000000, -0.2038245569916330158, -23.22168783648699986 ) ) ;
#14357 = ADVANCED_FACE ( 'NONE', ( #7447 ), #4477, .T. ) ;
#14358 = DIRECTION ( 'NONE',  ( -1.000000000000000000, -1.541976423090494894E-16, 0.000000000000000000 ) ) ;
#14359 = CARTESIAN_POINT ( 'NONE',  ( -101.2743836264399988, 111.1741184958670061, -15.85886927678779834 ) ) ;
#14360 = DIRECTION ( 'NONE',  ( -0.000000000000000000, -0.000000000000000000, -1.000000000000000000 ) ) ;
#14361 = DIRECTION ( 'NONE',  ( -1.000000000000000000, 0.000000000000000000, 0.000000000000000000 ) ) ;
#14362 = PLANE ( 'NONE',  #12481 ) ;
#14363 = ORIENTED_EDGE ( 'NONE', *, *, #11415, .F. ) ;
#14364 = CARTESIAN_POINT ( 'NONE',  ( -1.006616814747114065E-29, -2.568816543514387226E-44, 0.000000000000000000 ) ) ;
#14365 = EDGE_CURVE ( 'NONE', #14499, #6301, #9834, .T. ) ;
#14366 = EDGE_LOOP ( 'NONE', ( #949, #11588, #3802, #1026 ) ) ;
#14367 = EDGE_LOOP ( 'NONE', ( #7442, #10702, #2697, #5303 ) ) ;
#14368 = ORIENTED_EDGE ( 'NONE', *, *, #11121, .F. ) ;
#14369 = EDGE_CURVE ( 'NONE', #913, #11018, #524, .T. ) ;
#14370 = EDGE_CURVE ( 'NONE', #11286, #1855, #10929, .T. ) ;
#14371 = CARTESIAN_POINT ( 'NONE',  ( 2.684023608889491985, -1.139838562373123310, -3.272901415737858422 ) ) ;
#14372 = CARTESIAN_POINT ( 'NONE',  ( 6.205964732515537312E-15, 4.927357795815634489, 0.000000000000000000 ) ) ;
#14373 = FACE_OUTER_BOUND ( 'NONE', #9151, .T. ) ;
#14374 = CYLINDRICAL_SURFACE ( 'NONE', #2875, 4.499999999999997335 ) ;
#14375 = DIRECTION ( 'NONE',  ( -1.000000000000000000, 0.000000000000000000, 0.000000000000000000 ) ) ;
#14376 = DIRECTION ( 'NONE',  ( 0.000000000000000000, 0.000000000000000000, -1.000000000000000000 ) ) ;
#14377 = ORIENTED_EDGE ( 'NONE', *, *, #5717, .F. ) ;
#14378 = CYLINDRICAL_SURFACE ( 'NONE', #4634, 0.6000000000000000888 ) ;
#14379 = APPLICATION_PROTOCOL_DEFINITION ( 'draft international standard', 'automotive_design', 1998, #11997 ) ;
#14380 = ORIENTED_EDGE ( 'NONE', *, *, #6040, .T. ) ;
#14381 = CARTESIAN_POINT ( 'NONE',  ( -3.849008435184475996, -3.468750000000023093, -0.7641557335396481632 ) ) ;
#14382 = ORIENTED_EDGE ( 'NONE', *, *, #5565, .F. ) ;
#14383 = CARTESIAN_POINT ( 'NONE',  ( -2.441443777772203561, -1.225625000000065912, 2.973322847374053612 ) ) ;
#14384 = DIRECTION ( 'NONE',  ( -0.08715574274766157981, 1.084202172485503818E-16, 0.9961946980917452121 ) ) ;
#14385 = TOROIDAL_SURFACE ( 'NONE', #7950, 1.200000000000000178, 0.6000000000000000888 ) ;
#14386 = DIRECTION ( 'NONE',  ( -1.000000000000000000, 0.000000000000000000, 0.000000000000000000 ) ) ;
#14387 = FACE_OUTER_BOUND ( 'NONE', #11821, .T. ) ;
#14388 = CARTESIAN_POINT ( 'NONE',  ( 0.000000000000000000, 1.507583120841093915E-15, -56.77834603255778489 ) ) ;
#14389 = CARTESIAN_POINT ( 'NONE',  ( -1.096602777094355814E-14, 4.297149196226271783, 0.000000000000000000 ) ) ;
#14390 = ORIENTED_EDGE ( 'NONE', *, *, #11612, .F. ) ;
#14391 = DIRECTION ( 'NONE',  ( 0.000000000000000000, 0.000000000000000000, -1.000000000000000000 ) ) ;
#14392 = DIRECTION ( 'NONE',  ( 1.000000000000000000, 0.000000000000000000, 0.000000000000000000 ) ) ;
#14393 = ORIENTED_EDGE ( 'NONE', *, *, #9335, .T. ) ;
#14394 = LINE ( 'NONE', #3783, #4322 ) ;
#14395 = CARTESIAN_POINT ( 'NONE',  ( -3.335258087793214088, -3.022499999999893827, -1.380066378191329379 ) ) ;
#14396 = EDGE_LOOP ( 'NONE', ( #12512, #10545 ) ) ;
#14397 = EDGE_LOOP ( 'NONE', ( #3436, #12376 ) ) ;
#14398 = ORIENTED_EDGE ( 'NONE', *, *, #8789, .T. ) ;
#14399 = CIRCLE ( 'NONE', #7731, 2.500000000000002220 ) ;
#14400 = CARTESIAN_POINT ( 'NONE',  ( -86.77438362644001302, 99.17411849586700612, -152.4984795835769944 ) ) ;
#14401 =( GEOMETRIC_REPRESENTATION_CONTEXT ( 3 ) GLOBAL_UNCERTAINTY_ASSIGNED_CONTEXT ( ( #3904 ) ) GLOBAL_UNIT_ASSIGNED_CONTEXT ( ( #13130, #14051, #2252 ) ) REPRESENTATION_CONTEXT ( 'NONE', 'WORKASPACE' ) );
#14402 = CARTESIAN_POINT ( 'NONE',  ( -3.412007067234435809, -5.260309433033398818, -0.7367663078464588011 ) ) ;
#14403 = AXIS2_PLACEMENT_3D ( 'NONE', #5110, #9824, #3935 ) ;
#14404 = EDGE_CURVE ( 'NONE', #587, #9170, #6512, .T. ) ;
#14405 = CARTESIAN_POINT ( 'NONE',  ( -69.77438362644001302, 82.17411849586700612, -112.9984795835769944 ) ) ;
#14406 = CARTESIAN_POINT ( 'NONE',  ( -88.81638362644100937, 97.99516924618178848, -147.9984795835769944 ) ) ;
#14407 = FACE_BOUND ( 'NONE', #12256, .T. ) ;
#14408 = DIRECTION ( 'NONE',  ( 0.000000000000000000, 0.7547095802227716810, 0.6560590289905077199 ) ) ;
#14409 = EDGE_CURVE ( 'NONE', #486, #12362, #6250, .T. ) ;
#14410 = CARTESIAN_POINT ( 'NONE',  ( 2.950365215318619949, -3.491249999999835651, 1.969791294043586660 ) ) ;
#14411 = CARTESIAN_POINT ( 'NONE',  ( 35.35543536254876074, -19.31989681812820692, 6.000000000000000000 ) ) ;
#14412 = AXIS2_PLACEMENT_3D ( 'NONE', #3484, #15265, #8147 ) ;
#14413 = ORIENTED_EDGE ( 'NONE', *, *, #2817, .F. ) ;
#14414 = LINE ( 'NONE', #10867, #11980 ) ;
#14415 = VERTEX_POINT ( 'NONE', #594 ) ;
#14416 =( GEOMETRIC_REPRESENTATION_CONTEXT ( 3 ) GLOBAL_UNCERTAINTY_ASSIGNED_CONTEXT ( ( #11343 ) ) GLOBAL_UNIT_ASSIGNED_CONTEXT ( ( #10918, #10997, #2931 ) ) REPRESENTATION_CONTEXT ( 'NONE', 'WORKASPACE' ) );
#14417 = SHAPE_REPRESENTATION ( 'Part1', ( #285 ), #8229 ) ;
#14418 = EDGE_LOOP ( 'NONE', ( #11387, #11971, #11033, #2729, #14438, #14628 ) ) ;
#14419 = ORIENTED_EDGE ( 'NONE', *, *, #12834, .F. ) ;
#14420 = ORIENTED_EDGE ( 'NONE', *, *, #5948, .T. ) ;
#14421 = AXIS2_PLACEMENT_3D ( 'NONE', #7469, #3964, #11959 ) ;
#14422 = DIRECTION ( 'NONE',  ( 1.000000000000000000, 0.000000000000000000, 0.000000000000000000 ) ) ;
#14423 = COLOUR_RGB ( '', 0.40784314, 0.44705882, 0.49803922) ;
#14424 = DIRECTION ( 'NONE',  ( 0.8660254037844387076, 0.4999999999999998890, 0.000000000000000000 ) ) ;
#14425 = EDGE_CURVE ( 'NONE', #9494, #8700, #11927, .T. ) ;
#14426 = DIRECTION ( 'NONE',  ( -1.000000000000000000, 0.000000000000000000, -0.000000000000000000 ) ) ;
#14427 = DIRECTION ( 'NONE',  ( 0.1816390095645149805, 0.000000000000000000, -0.9833652781161342782 ) ) ;
#14428 = EDGE_CURVE ( 'NONE', #11930, #7225, #4991, .T. ) ;
#14429 = FACE_OUTER_BOUND ( 'NONE', #9685, .T. ) ;
#14430 = FACE_OUTER_BOUND ( 'NONE', #9988, .T. ) ;
#14431 = CARTESIAN_POINT ( 'NONE',  ( 15.50000000000000000, -1.037157890325000054, 26.50000000000000000 ) ) ;
#14432 = CARTESIAN_POINT ( 'NONE',  ( -63.28565528768381654, 67.29799558322736175, -81.84847958357697451 ) ) ;
#14433 = VECTOR ( 'NONE', #12187, 999.9999999999998863 ) ;
#14434 = DIRECTION ( 'NONE',  ( 0.000000000000000000, -0.000000000000000000, 1.000000000000000000 ) ) ;
#14435 = CARTESIAN_POINT ( 'NONE',  ( -86.77438362644100778, 101.5320169952374414, -147.9984795835769944 ) ) ;
#14436 = ORIENTED_EDGE ( 'NONE', *, *, #7929, .T. ) ;
#14437 = DIRECTION ( 'NONE',  ( 0.000000000000000000, 0.000000000000000000, 1.000000000000000000 ) ) ;
#14438 = ORIENTED_EDGE ( 'NONE', *, *, #10272, .T. ) ;
#14439 = CIRCLE ( 'NONE', #321, 1.199999999999711520 ) ;
#14440 = EDGE_LOOP ( 'NONE', ( #426, #3531 ) ) ;
#14441 = ORIENTED_EDGE ( 'NONE', *, *, #13985, .F. ) ;
#14442 = CARTESIAN_POINT ( 'NONE',  ( -1.266249875242109635, -5.272499999999733511, 3.060236832100307058 ) ) ;
#14443 = EDGE_CURVE ( 'NONE', #8857, #6323, #8442, .T. ) ;
#14444 = CARTESIAN_POINT ( 'NONE',  ( -35.58670980944424400, 5.000000000000001776, 133.4783111191910621 ) ) ;
#14445 = AXIS2_PLACEMENT_3D ( 'NONE', #1665, #14453, #12139 ) ;
#14446 = CARTESIAN_POINT ( 'NONE',  ( 2.372463320875326520, -0.8429635623729573313, 3.552691932206611281 ) ) ;
#14447 = AXIS2_PLACEMENT_3D ( 'NONE', #13449, #11339, #7559 ) ;
#14448 = CARTESIAN_POINT ( 'NONE',  ( -3.127990687458614971, 2.260916199238037239E-16, 54.09781049769389938 ) ) ;
#14449 = CARTESIAN_POINT ( 'NONE',  ( -15.50000000000000000, -0.2038245569916614930, 21.05662432702600029 ) ) ;
#14450 = EDGE_CURVE ( 'NONE', #10494, #4413, #372, .T. ) ;
#14451 = DIRECTION ( 'NONE',  ( 0.000000000000000000, 0.000000000000000000, -1.000000000000000000 ) ) ;
#14452 = VECTOR ( 'NONE', #9305, 1000.000000000000000 ) ;
#14453 = DIRECTION ( 'NONE',  ( 0.000000000000000000, 0.000000000000000000, 1.000000000000000000 ) ) ;
#14454 = EDGE_CURVE ( 'NONE', #3974, #4383, #25, .T. ) ;
#14455 = CARTESIAN_POINT ( 'NONE',  ( -80.52077156573417938, 60.67411849586702743, -79.59847958357700293 ) ) ;
#14456 = EDGE_CURVE ( 'NONE', #8210, #2658, #7526, .T. ) ;
#14457 = EDGE_LOOP ( 'NONE', ( #1240, #14178, #895, #3900, #1573, #13693, #752, #8973, #5454 ) ) ;
#14458 = DIRECTION ( 'NONE',  ( 1.000000000000000000, 0.000000000000000000, 0.000000000000000000 ) ) ;
#14459 = CIRCLE ( 'NONE', #14218, 2.700000000000001066 ) ;
#14460 = VECTOR ( 'NONE', #9989, 1000.000000000000000 ) ;
#14461 = CONTEXT_DEPENDENT_SHAPE_REPRESENTATION ( #9600, #9905 ) ;
#14462 = ORIENTED_EDGE ( 'NONE', *, *, #9121, .F. ) ;
#14463 = FILL_AREA_STYLE ('',( #261 ) ) ;
#14464 = ADVANCED_FACE ( 'NONE', ( #12245 ), #1615, .F. ) ;
#14465 = CARTESIAN_POINT ( 'NONE',  ( 3.553279128418493915, -4.062500000000332179, -1.470728592776388455 ) ) ;
#14466 = ORIENTED_EDGE ( 'NONE', *, *, #11625, .T. ) ;
#14467 = CARTESIAN_POINT ( 'NONE',  ( 3.776578263379590350, -4.030463562373150843, -0.7501819099998634499 ) ) ;
#14468 = CARTESIAN_POINT ( 'NONE',  ( -1.487946254897619447, -0.8975000000000187272, -3.594883137563858355 ) ) ;
#14469 = CIRCLE ( 'NONE', #6073, 3.749999999999996447 ) ;
#14470 = EDGE_CURVE ( 'NONE', #4691, #12791, #7957, .T. ) ;
#14471 = LINE ( 'NONE', #6274, #3369 ) ;
#14472 = DIRECTION ( 'NONE',  ( -1.000000000000000000, 0.000000000000000000, 0.000000000000000000 ) ) ;
#14473 = PLANE ( 'NONE',  #104 ) ;
#14474 = FACE_OUTER_BOUND ( 'NONE', #7503, .T. ) ;
#14475 = DIRECTION ( 'NONE',  ( 0.000000000000000000, 0.000000000000000000, 1.000000000000000000 ) ) ;
#14476 = DIRECTION ( 'NONE',  ( 1.000000000000000000, 0.000000000000000000, 0.000000000000000000 ) ) ;
#14477 = ORIENTED_EDGE ( 'NONE', *, *, #6325, .T. ) ;
#14478 = LINE ( 'NONE', #2302, #11753 ) ;
#14479 = VECTOR ( 'NONE', #4292, 1000.000000000000114 ) ;
#14480 = ORIENTED_EDGE ( 'NONE', *, *, #11799, .F. ) ;
#14481 = CARTESIAN_POINT ( 'NONE',  ( -69.77438362644100778, 82.17411849586699191, -67.49847958357700861 ) ) ;
#14482 = CARTESIAN_POINT ( 'NONE',  ( -1.707523105661755025, -2.913124999999936904, -3.196535590052165254 ) ) ;
#14483 = ORIENTED_EDGE ( 'NONE', *, *, #8021, .T. ) ;
#14484 = EDGE_LOOP ( 'NONE', ( #7155, #3135 ) ) ;
#14485 = CARTESIAN_POINT ( 'NONE',  ( -77.52077156573416516, 60.67411849586702743, -73.34256232478206528 ) ) ;
#14486 = CARTESIAN_POINT ( 'NONE',  ( -0.1886744959232814767, -5.170134308371691745, -3.603086115839904569 ) ) ;
#14487 = DIRECTION ( 'NONE',  ( 0.000000000000000000, 1.000000000000000000, 0.000000000000000000 ) ) ;
#14488 = VECTOR ( 'NONE', #2921, 1000.000000000000114 ) ;
#14489 = CARTESIAN_POINT ( 'NONE',  ( -2.397583379056643427, -0.4995676945082651588, -3.461308205639501256 ) ) ;
#14490 = CARTESIAN_POINT ( 'NONE',  ( 15.29633693294940677, -0.2717122460100966919, -21.17420925361164308 ) ) ;
#14491 = AXIS2_PLACEMENT_3D ( 'NONE', #1330, #10482, #15209 ) ;
#14492 = LINE ( 'NONE', #13352, #6599 ) ;
#14493 = DIRECTION ( 'NONE',  ( 1.000000000000000000, 0.000000000000000000, 0.000000000000000000 ) ) ;
#14494 = ORIENTED_EDGE ( 'NONE', *, *, #5140, .F. ) ;
#14495 = CARTESIAN_POINT ( 'NONE',  ( -52.77438362643999881, 65.17411849586700612, -79.59847958357700293 ) ) ;
#14496 = ORIENTED_EDGE ( 'NONE', *, *, #10278, .T. ) ;
#14497 = ORIENTED_EDGE ( 'NONE', *, *, #13490, .T. ) ;
#14498 = ORIENTED_EDGE ( 'NONE', *, *, #8169, .F. ) ;
#14499 = VERTEX_POINT ( 'NONE', #15084 ) ;
#14500 = DIRECTION ( 'NONE',  ( 0.000000000000000000, 1.000000000000000000, 0.000000000000000000 ) ) ;
#14501 = VECTOR ( 'NONE', #3231, 1000.000000000000000 ) ;
#14502 = CARTESIAN_POINT ( 'NONE',  ( 3.244093391032126572, -2.506875000000020837, 1.732468392772068544 ) ) ;
#14503 = EDGE_CURVE ( 'NONE', #2640, #6920, #8039, .T. ) ;
#14504 = DIRECTION ( 'NONE',  ( -1.000000000000000000, -2.505711687522054122E-15, 0.000000000000000000 ) ) ;
#14505 = CARTESIAN_POINT ( 'NONE',  ( -3.849008435184475996, -3.468750000000023093, -0.7641557335396481632 ) ) ;
#14506 = PLANE ( 'NONE',  #1043 ) ;
#14507 = DIRECTION ( 'NONE',  ( 0.4999999999999827360, 0.000000000000000000, 0.8660254037844485886 ) ) ;
#14508 = DIRECTION ( 'NONE',  ( 1.000000000000000000, 0.000000000000000000, 0.000000000000000000 ) ) ;
#14509 = DIRECTION ( 'NONE',  ( -1.000000000000000000, 0.000000000000000000, 0.000000000000000000 ) ) ;
#14510 = VECTOR ( 'NONE', #11993, 1000.000000000000000 ) ;
#14511 = DIRECTION ( 'NONE',  ( -0.000000000000000000, 1.000000000000000000, -0.000000000000000000 ) ) ;
#14512 = PLANE ( 'NONE',  #1388 ) ;
#14513 = CARTESIAN_POINT ( 'NONE',  ( -69.77438362644001302, 82.17411849586700612, -82.44847958357698303 ) ) ;
#14514 = CONICAL_SURFACE ( 'NONE', #9052, 1732.050807568789651, 1.047197551196575871 ) ;
#14515 = EDGE_LOOP ( 'NONE', ( #723, #5384, #6771, #9644 ) ) ;
#14516 = DIRECTION ( 'NONE',  ( 0.000000000000000000, 0.000000000000000000, -1.000000000000000000 ) ) ;
#14517 = ORIENTED_EDGE ( 'NONE', *, *, #1838, .T. ) ;
#14518 = ORIENTED_EDGE ( 'NONE', *, *, #14565, .T. ) ;
#14519 = CARTESIAN_POINT ( 'NONE',  ( 2.709518412118975483, -5.678749999999861409, -1.809455179588199014 ) ) ;
#14520 = EDGE_CURVE ( 'NONE', #6682, #10550, #6817, .T. ) ;
#14521 = CARTESIAN_POINT ( 'NONE',  ( 11.10026251182900481, -85.69524470659703752, 69.17694817598116686 ) ) ;
#14522 = VECTOR ( 'NONE', #2093, 1000.000000000000000 ) ;
#14523 = CARTESIAN_POINT ( 'NONE',  ( -2.103997734759339711, -5.225624999999808118, 2.565685703212198021 ) ) ;
#14524 = ADVANCED_FACE ( 'NONE', ( #2146, #6893 ), #7892, .T. ) ;
#14525 = CIRCLE ( 'NONE', #2641, 2.750000000000002665 ) ;
#14526 = CARTESIAN_POINT ( 'NONE',  ( 21.98164641901421135, -11.40000029085424238, -0.3335879563140091153 ) ) ;
#14527 = DIRECTION ( 'NONE',  ( -0.000000000000000000, 1.000000000000000000, 0.000000000000000000 ) ) ;
#14528 = DIRECTION ( 'NONE',  ( -1.000000000000000000, 0.000000000000000000, 0.000000000000000000 ) ) ;
#14529 = DIRECTION ( 'NONE',  ( 1.000000000000000000, -0.000000000000000000, 0.000000000000000000 ) ) ;
#14530 = DIRECTION ( 'NONE',  ( 0.000000000000000000, 0.000000000000000000, 1.000000000000000000 ) ) ;
#14531 = CARTESIAN_POINT ( 'NONE',  ( 15.50000000000000000, -0.1999999999999999556, 21.05000000000000426 ) ) ;
#14532 = ORIENTED_EDGE ( 'NONE', *, *, #3335, .F. ) ;
#14533 = CARTESIAN_POINT ( 'NONE',  ( -62.02799568714584666, 59.67411849586701322, -15.85886927678779834 ) ) ;
#14534 = CIRCLE ( 'NONE', #1164, 5.499999999999998224 ) ;
#14535 = CONTEXT_DEPENDENT_SHAPE_REPRESENTATION ( #2178, #4621 ) ;
#14536 = EDGE_CURVE ( 'NONE', #12493, #263, #5659, .T. ) ;
#14537 = ORIENTED_EDGE ( 'NONE', *, *, #11349, .T. ) ;
#14538 = DIRECTION ( 'NONE',  ( -6.982962677686266711E-15, -6.579622859988665673E-30, -1.000000000000000000 ) ) ;
#14539 = CARTESIAN_POINT ( 'NONE',  ( -3.970076885172157066, -2.531249999999920064, 0.7911966920917139490 ) ) ;
#14540 = ORIENTED_EDGE ( 'NONE', *, *, #8593, .T. ) ;
#14541 = CARTESIAN_POINT ( 'NONE',  ( 1.742702564072879046, -5.171088562373163278, -3.263254631422885854 ) ) ;
#14542 = ADVANCED_FACE ( 'NONE', ( #11536 ), #10358, .T. ) ;
#14543 = CARTESIAN_POINT ( 'NONE',  ( 3.432145566543734372, -0.5044392315027305118, 1.902605341171852427 ) ) ;
#14544 = LINE ( 'NONE', #3926, #5845 ) ;
#14545 = AXIS2_PLACEMENT_3D ( 'NONE', #13643, #1051, #12931 ) ;
#14546 = LINE ( 'NONE', #6495, #2790 ) ;
#14547 = FACE_OUTER_BOUND ( 'NONE', #4609, .T. ) ;
#14548 = EDGE_CURVE ( 'NONE', #14010, #3959, #5734, .T. ) ;
#14549 = DIRECTION ( 'NONE',  ( 0.000000000000000000, 0.000000000000000000, -1.000000000000000000 ) ) ;
#14550 = DIRECTION ( 'NONE',  ( 0.8660254037844383745, -0.5000000000000003331, 0.000000000000000000 ) ) ;
#14551 = CARTESIAN_POINT ( 'NONE',  ( -52.77438362644100067, 99.17411849586700612, -145.4984795835769944 ) ) ;
#14552 = DIRECTION ( 'NONE',  ( 0.000000000000000000, 1.000000000000000000, 0.000000000000000000 ) ) ;
#14553 = CARTESIAN_POINT ( 'NONE',  ( 40.52020888806953991, 0.000000000000000000, 0.000000000000000000 ) ) ;
#14554 = ORIENTED_EDGE ( 'NONE', *, *, #2783, .F. ) ;
#14555 = EDGE_LOOP ( 'NONE', ( #8093, #7153, #9683 ) ) ;
#14556 = DIRECTION ( 'NONE',  ( 1.000000000000000000, 0.000000000000000000, 0.000000000000000000 ) ) ;
#14557 = ADVANCED_FACE ( 'NONE', ( #11611, #4177 ), #8901, .T. ) ;
#14558 = ORIENTED_EDGE ( 'NONE', *, *, #11337, .F. ) ;
#14559 = CONICAL_SURFACE ( 'NONE', #2673, 3.750000000000003553, 0.7853981633974476129 ) ;
#14560 = DIRECTION ( 'NONE',  ( 0.000000000000000000, -0.8571673007021106683, 0.5150380749100569311 ) ) ;
#14561 = CARTESIAN_POINT ( 'NONE',  ( -0.0009180086920682582752, -3.334999999999859632, 3.568205616840287142 ) ) ;
#14562 = ORIENTED_EDGE ( 'NONE', *, *, #14640, .T. ) ;
#14563 = ORIENTED_EDGE ( 'NONE', *, *, #13059, .F. ) ;
#14564 = EDGE_CURVE ( 'NONE', #6473, #5823, #13641, .T. ) ;
#14565 = EDGE_CURVE ( 'NONE', #9704, #1058, #9191, .T. ) ;
#14566 = CARTESIAN_POINT ( 'NONE',  ( -15.50000000000000000, -0.1999999999999999556, -22.50000000000000000 ) ) ;
#14567 = CARTESIAN_POINT ( 'NONE',  ( -3.198284477310383789, -5.245703666927238551, -1.445171886050707011 ) ) ;
#14568 = DIRECTION ( 'NONE',  ( 0.000000000000000000, -0.000000000000000000, 1.000000000000000000 ) ) ;
#14569 = AXIS2_PLACEMENT_3D ( 'NONE', #15108, #13741, #10456 ) ;
#14570 = CARTESIAN_POINT ( 'NONE',  ( -23.24999999999999289, -10.00000000000000000, 27.00000000000000000 ) ) ;
#14571 = DIRECTION ( 'NONE',  ( 0.000000000000000000, 0.000000000000000000, -1.000000000000000000 ) ) ;
#14572 = LINE ( 'NONE', #5043, #4544 ) ;
#14573 = VERTEX_POINT ( 'NONE', #11304 ) ;
#14574 = PLANE ( 'NONE',  #8262 ) ;
#14575 = VERTEX_POINT ( 'NONE', #1839 ) ;
#14576 = VERTEX_POINT ( 'NONE', #675 ) ;
#14577 = ORIENTED_EDGE ( 'NONE', *, *, #6805, .T. ) ;
#14578 = ORIENTED_EDGE ( 'NONE', *, *, #6444, .F. ) ;
#14579 = ORIENTED_EDGE ( 'NONE', *, *, #13535, .T. ) ;
#14580 = AXIS2_PLACEMENT_3D ( 'NONE', #9582, #5810, #8277 ) ;
#14581 = DIRECTION ( 'NONE',  ( 0.000000000000000000, 1.000000000000000000, 0.000000000000000000 ) ) ;
#14582 = CARTESIAN_POINT ( 'NONE',  ( -86.77438362644001302, 65.17411849586700612, -152.4984795835769944 ) ) ;
#14583 = CARTESIAN_POINT ( 'NONE',  ( 1.514604053328734823, -3.187500000000060396, -3.660349086209866876 ) ) ;
#14584 = DIRECTION ( 'NONE',  ( 0.000000000000000000, 0.000000000000000000, 1.000000000000000000 ) ) ;
#14585 = CARTESIAN_POINT ( 'NONE',  ( 0.8667276783654334071, 2.116104415309936157E-15, 4.500000000000000000 ) ) ;
#14586 = CARTESIAN_POINT ( 'NONE',  ( -4.342069816296838525, 2.307268873417408273, -1.479314468162620466 ) ) ;
#14587 = CARTESIAN_POINT ( 'NONE',  ( -56.85838362643999488, 65.17411849586700612, -147.9984795835769944 ) ) ;
#14588 = CARTESIAN_POINT ( 'NONE',  ( 15.50000000000000000, -1.037157890325000054, 19.00000000000000000 ) ) ;
#14589 = CARTESIAN_POINT ( 'NONE',  ( 1.274862231047225439E-15, -0.4995676945082591081, 0.000000000000000000 ) ) ;
#14590 = CARTESIAN_POINT ( 'NONE',  ( 16.75000000000000000, -0.2714405302574892098, -22.98746066354537376 ) ) ;
#14591 = VECTOR ( 'NONE', #12317, 1000.000000000000000 ) ;
#14592 = ORIENTED_EDGE ( 'NONE', *, *, #3421, .F. ) ;
#14593 = CARTESIAN_POINT ( 'NONE',  ( -55.27438362643999881, 65.17411849586700612, -145.2984795835770058 ) ) ;
#14594 = ORIENTED_EDGE ( 'NONE', *, *, #12379, .F. ) ;
#14595 = VERTEX_POINT ( 'NONE', #5425 ) ;
#14596 = ORIENTED_EDGE ( 'NONE', *, *, #2953, .F. ) ;
#14597 = CARTESIAN_POINT ( 'NONE',  ( -0.6299995022919476773, -5.866249999999999964, -3.171388681290751688 ) ) ;
#14598 = DIRECTION ( 'NONE',  ( -1.000000000000000000, 0.000000000000000000, 0.000000000000000000 ) ) ;
#14599 = PLANE ( 'NONE',  #616 ) ;
#14600 = CARTESIAN_POINT ( 'NONE',  ( -90.52438362643999881, 65.17411849586700612, -150.4984795835770228 ) ) ;
#14601 = DIRECTION ( 'NONE',  ( -0.000000000000000000, 1.000000000000000000, -0.000000000000000000 ) ) ;
#14602 = DIRECTION ( 'NONE',  ( -1.000000000000000000, 0.000000000000000000, 0.000000000000000000 ) ) ;
#14603 = DIRECTION ( 'NONE',  ( 0.9961946980917452121, -3.779777825264101491E-17, 0.08715574274766160756 ) ) ;
#14604 = EDGE_CURVE ( 'NONE', #15148, #11761, #9935, .T. ) ;
#14605 = DIRECTION ( 'NONE',  ( -1.000000000000000000, 0.000000000000000000, 0.000000000000000000 ) ) ;
#14606 = ORIENTED_EDGE ( 'NONE', *, *, #13014, .T. ) ;
#14607 = FACE_OUTER_BOUND ( 'NONE', #12383, .T. ) ;
#14608 = EDGE_CURVE ( 'NONE', #10624, #3281, #6967, .T. ) ;
#14609 = ORIENTED_EDGE ( 'NONE', *, *, #4778, .F. ) ;
#14610 = FILL_AREA_STYLE ('',( #1674 ) ) ;
#14611 = CARTESIAN_POINT ( 'NONE',  ( 3.325473450044490242, -2.906249999999835243, 2.220260485081660740 ) ) ;
#14612 = ORIENTED_EDGE ( 'NONE', *, *, #1287, .T. ) ;
#14613 = CARTESIAN_POINT ( 'NONE',  ( -86.77438362644001302, 99.17411849586700612, -152.4984795835769944 ) ) ;
#14614 = CARTESIAN_POINT ( 'NONE',  ( 15.14695642955105193, -1.094824204497501265E-15, 22.92302504315390621 ) ) ;
#14615 = DIRECTION ( 'NONE',  ( -9.422394424380278809E-16, 1.000000000000000000, -0.000000000000000000 ) ) ;
#14616 = EDGE_CURVE ( 'NONE', #11643, #11128, #4440, .T. ) ;
#14617 = LINE ( 'NONE', #11652, #12254 ) ;
#14618 = DIRECTION ( 'NONE',  ( 2.065146995210485003E-17, 4.251773225433349175E-17, 1.000000000000000000 ) ) ;
#14619 = CARTESIAN_POINT ( 'NONE',  ( -86.77438362644100778, 96.81621999649657084, -147.9984795835769944 ) ) ;
#14620 = DIRECTION ( 'NONE',  ( 0.000000000000000000, 0.000000000000000000, 1.000000000000000000 ) ) ;
#14621 = CARTESIAN_POINT ( 'NONE',  ( 1.274862231047225439E-15, -0.4995676945082591081, 0.000000000000000000 ) ) ;
#14622 = EDGE_CURVE ( 'NONE', #14101, #4356, #10169, .T. ) ;
#14623 = CYLINDRICAL_SURFACE ( 'NONE', #2026, 2.000000000000001776 ) ;
#14624 = VERTEX_POINT ( 'NONE', #5807 ) ;
#14625 = ORIENTED_EDGE ( 'NONE', *, *, #2908, .T. ) ;
#14626 = CARTESIAN_POINT ( 'NONE',  ( 16.75000000000000000, -2.500000000000000000, 23.22168783648699986 ) ) ;
#14627 = CARTESIAN_POINT ( 'NONE',  ( -3.717546150574278840, -2.069374999999891607, -0.3671215460811527720 ) ) ;
#14628 = ORIENTED_EDGE ( 'NONE', *, *, #5748, .T. ) ;
#14629 = EDGE_CURVE ( 'NONE', #4356, #14101, #11425, .T. ) ;
#14630 = EDGE_CURVE ( 'NONE', #10105, #3491, #1283, .T. ) ;
#14631 = DIRECTION ( 'NONE',  ( -2.551930889570660354E-15, 1.000000000000000000, 0.000000000000000000 ) ) ;
#14632 = AXIS2_PLACEMENT_3D ( 'NONE', #7027, #13547, #257 ) ;
#14633 = CARTESIAN_POINT ( 'NONE',  ( 2.252671702316018543, -5.120840197140201333, -2.900062017644191581 ) ) ;
#14634 = ADVANCED_FACE ( 'NONE', ( #14238 ), #11765, .F. ) ;
#14635 = DIRECTION ( 'NONE',  ( 0.000000000000000000, 1.000000000000000000, 0.000000000000000000 ) ) ;
#14636 = AXIS2_PLACEMENT_3D ( 'NONE', #6218, #1537, #5265 ) ;
#14637 = DIRECTION ( 'NONE',  ( -0.000000000000000000, 1.000000000000000000, -0.000000000000000000 ) ) ;
#14638 = DIRECTION ( 'NONE',  ( 0.000000000000000000, 0.000000000000000000, 1.000000000000000000 ) ) ;
#14639 = FACE_OUTER_BOUND ( 'NONE', #11357, .T. ) ;
#14640 = EDGE_CURVE ( 'NONE', #11342, #1533, #7199, .T. ) ;
#14641 = CARTESIAN_POINT ( 'NONE',  ( 22.58164641901421632, 11.99999970914576330, -11.73358795631400753 ) ) ;
#14642 = EDGE_CURVE ( 'NONE', #1405, #3140, #265, .T. ) ;
#14643 = ORIENTED_EDGE ( 'NONE', *, *, #3375, .F. ) ;
#14644 = PLANE ( 'NONE',  #11745 ) ;
#14645 = ORIENTED_EDGE ( 'NONE', *, *, #10564, .F. ) ;
#14646 = AXIS2_PLACEMENT_3D ( 'NONE', #4458, #10412, #3371 ) ;
#14647 = ORIENTED_EDGE ( 'NONE', *, *, #7749, .F. ) ;
#14648 = ORIENTED_EDGE ( 'NONE', *, *, #9344, .F. ) ;
#14649 = ORIENTED_EDGE ( 'NONE', *, *, #9024, .F. ) ;
#14650 = ORIENTED_EDGE ( 'NONE', *, *, #6304, .T. ) ;
#14651 = AXIS2_PLACEMENT_3D ( 'NONE', #12991, #4845, #11896 ) ;
#14652 = CARTESIAN_POINT ( 'NONE',  ( -65.78565528768382364, 67.29799558322736175, -81.84847958357697451 ) ) ;
#14653 = EDGE_CURVE ( 'NONE', #16, #13148, #3461, .T. ) ;
#14654 = VECTOR ( 'NONE', #11144, 999.9999999999998863 ) ;
#14655 = CARTESIAN_POINT ( 'NONE',  ( -1.750120246539625946, -2.256875000000012843, 3.272202384321437840 ) ) ;
#14656 = CARTESIAN_POINT ( 'NONE',  ( 15.50000000000000000, -1.037157890325000054, 22.50000000000000000 ) ) ;
#14657 = CARTESIAN_POINT ( 'NONE',  ( -3.920035875790600421, -3.499999999999977796, -0.001028343392498549860 ) ) ;
#14658 = CARTESIAN_POINT ( 'NONE',  ( 14.24999999999999822, -0.3152037684892591285, -22.25410949791979220 ) ) ;
#14659 = EDGE_CURVE ( 'NONE', #13263, #11097, #2291, .T. ) ;
#14660 = DIRECTION ( 'NONE',  ( -9.422394424380278809E-16, 1.000000000000000000, -0.000000000000000000 ) ) ;
#14661 = VECTOR ( 'NONE', #941, 1000.000000000000000 ) ;
#14662 = CARTESIAN_POINT ( 'NONE',  ( -5.196152422706636465, 2.374999999999986677, -8.561039196169309507E-16 ) ) ;
#14663 = CARTESIAN_POINT ( 'NONE',  ( -82.52438362643998460, 65.17411849586700612, -149.9984795835770228 ) ) ;
#14664 = CARTESIAN_POINT ( 'NONE',  ( -15.50000000000000000, 0.000000000000000000, 18.50000000000000000 ) ) ;
#14665 = DIRECTION ( 'NONE',  ( -1.287488025362404182E-15, -1.000000000000000000, 0.000000000000000000 ) ) ;
#14666 = CARTESIAN_POINT ( 'NONE',  ( 16.75000000000000355, -0.2715193793361411756, -22.01281590054916038 ) ) ;
#14667 = VECTOR ( 'NONE', #9232, 999.9999999999998863 ) ;
#14668 = ORIENTED_EDGE ( 'NONE', *, *, #1342, .T. ) ;
#14669 = DIRECTION ( 'NONE',  ( 0.000000000000000000, 0.000000000000000000, 1.000000000000000000 ) ) ;
#14670 = AXIS2_PLACEMENT_3D ( 'NONE', #815, #6953, #11673 ) ;
#14671 = ORIENTED_EDGE ( 'NONE', *, *, #1359, .T. ) ;
#14672 = ORIENTED_EDGE ( 'NONE', *, *, #3872, .F. ) ;
#14673 = ORIENTED_EDGE ( 'NONE', *, *, #13630, .T. ) ;
#14674 = DIRECTION ( 'NONE',  ( 0.000000000000000000, 0.000000000000000000, -1.000000000000000000 ) ) ;
#14675 = DIRECTION ( 'NONE',  ( 7.199281117894584284E-17, -0.7071067811865485719, -0.7071067811865465735 ) ) ;
#14676 = DIRECTION ( 'NONE',  ( -0.000000000000000000, 1.000000000000000000, -0.000000000000000000 ) ) ;
#14677 = DIRECTION ( 'NONE',  ( -0.000000000000000000, 1.000000000000000000, -0.000000000000000000 ) ) ;
#14678 = AXIS2_PLACEMENT_3D ( 'NONE', #9734, #8729, #9964 ) ;
#14679 = CARTESIAN_POINT ( 'NONE',  ( 2.937061643673781752, -5.103115294876279684, -2.234448363260541193 ) ) ;
#14680 = CARTESIAN_POINT ( 'NONE',  ( -16.94999999999999929, -0.2000000000000000111, 22.50000000000000000 ) ) ;
#14681 = CARTESIAN_POINT ( 'NONE',  ( -15.50000000000000000, -5.000000000000000000, 22.50000000000000000 ) ) ;
#14682 = CIRCLE ( 'NONE', #7025, 4.500000000000000888 ) ;
#14683 = CARTESIAN_POINT ( 'NONE',  ( -101.2743836264399988, 60.67411849586700612, -79.49847958357700861 ) ) ;
#14684 = VERTEX_POINT ( 'NONE', #875 ) ;
#14685 = CARTESIAN_POINT ( 'NONE',  ( -75.01311196519617397, 67.29799558322736175, -81.84847958357697451 ) ) ;
#14686 = VECTOR ( 'NONE', #8256, 1000.000000000000000 ) ;
#14687 = EDGE_LOOP ( 'NONE', ( #1999, #14578, #7543, #5069 ) ) ;
#14688 = CARTESIAN_POINT ( 'NONE',  ( -88.81638362644100937, 97.99516924618178848, -150.4984795835770228 ) ) ;
#14689 = CARTESIAN_POINT ( 'NONE',  ( -0.001059456894846966344, -2.749999999999859224, 4.019249942169077272 ) ) ;
#14690 = EDGE_LOOP ( 'NONE', ( #7764, #5552, #10676, #3100 ) ) ;
#14691 = AXIS2_PLACEMENT_3D ( 'NONE', #8304, #5995, #1235 ) ;
#14692 = CARTESIAN_POINT ( 'NONE',  ( -52.77438362644000591, 99.17411849586700612, -86.49847958357699440 ) ) ;
#14693 = EDGE_CURVE ( 'NONE', #10808, #12550, #13841, .T. ) ;
#14694 = CARTESIAN_POINT ( 'NONE',  ( -6.714472293954755422, -12.00000029085427578, 37.72291661448763733 ) ) ;
#14695 = CARTESIAN_POINT ( 'NONE',  ( 5.196152422706624918, 2.375000000000013323, -1.265134450516282343E-15 ) ) ;
#14696 = AXIS2_PLACEMENT_3D ( 'NONE', #12295, #13545, #3838 ) ;
#14697 = CARTESIAN_POINT ( 'NONE',  ( -15.50000000000000000, -1.037157890325000054, 22.50000000000000000 ) ) ;
#14698 = CARTESIAN_POINT ( 'NONE',  ( -53.27438362644000591, 82.17411849586700612, -150.4984795835769944 ) ) ;
#14699 = LINE ( 'NONE', #3073, #5368 ) ;
#14700 = CYLINDRICAL_SURFACE ( 'NONE', #7860, 16.06499999999999773 ) ;
#14701 = PLANE ( 'NONE',  #1280 ) ;
#14702 = VECTOR ( 'NONE', #1121, 1000.000000000000000 ) ;
#14703 = ORIENTED_EDGE ( 'NONE', *, *, #5194, .F. ) ;
#14704 = ORIENTED_EDGE ( 'NONE', *, *, #4800, .F. ) ;
#14705 = CYLINDRICAL_SURFACE ( 'NONE', #2835, 4.249999999999996447 ) ;
#14706 = CARTESIAN_POINT ( 'NONE',  ( -3.693744850241972522, -1.131875000000025722, 1.119430425315800282 ) ) ;
#14707 = ORIENTED_EDGE ( 'NONE', *, *, #6345, .F. ) ;
#14708 = AXIS2_PLACEMENT_3D ( 'NONE', #5986, #7064, #14181 ) ;
#14709 = EDGE_CURVE ( 'NONE', #9995, #12177, #4453, .T. ) ;
#14710 = AXIS2_PLACEMENT_3D ( 'NONE', #12480, #3086, #15014 ) ;
#14711 = EDGE_CURVE ( 'NONE', #3303, #9311, #797, .T. ) ;
#14712 = LINE ( 'NONE', #3948, #5407 ) ;
#14713 = LINE ( 'NONE', #10128, #8774 ) ;
#14714 = CARTESIAN_POINT ( 'NONE',  ( -0.6343012717231791830, -0.4995676945082608289, -4.116477779236263679 ) ) ;
#14715 = FACE_OUTER_BOUND ( 'NONE', #11741, .T. ) ;
#14716 = CARTESIAN_POINT ( 'NONE',  ( -14.24999999999999822, -0.3152037684892585179, -22.74589050208021135 ) ) ;
#14717 = CIRCLE ( 'NONE', #8035, 0.5000000000000000000 ) ;
#14718 = VECTOR ( 'NONE', #2865, 1000.000000000000114 ) ;
#14719 = CONICAL_SURFACE ( 'NONE', #9512, 3.749999999999996447, 0.7853981633974476129 ) ;
#14720 = CARTESIAN_POINT ( 'NONE',  ( -14.25000000000000000, -2.500000000000000000, 21.77831216351300014 ) ) ;
#14721 = EDGE_LOOP ( 'NONE', ( #15113, #9362, #11489, #13887 ) ) ;
#14722 = CARTESIAN_POINT ( 'NONE',  ( 16.33757311576526305, -0.3152598339554824047, -23.45980260912095616 ) ) ;
#14723 = EDGE_LOOP ( 'NONE', ( #15098, #11951, #9825, #10870 ) ) ;
#14724 = ORIENTED_EDGE ( 'NONE', *, *, #9593, .F. ) ;
#14725 = VERTEX_POINT ( 'NONE', #11589 ) ;
#14726 = VERTEX_POINT ( 'NONE', #6791 ) ;
#14727 = ADVANCED_FACE ( 'NONE', ( #8949, #727 ), #15064, .T. ) ;
#14728 = ORIENTED_EDGE ( 'NONE', *, *, #10095, .F. ) ;
#14729 = DIRECTION ( 'NONE',  ( 0.000000000000000000, 0.000000000000000000, -1.000000000000000000 ) ) ;
#14730 = CARTESIAN_POINT ( 'NONE',  ( 3.779448512589415721, -1.600625000000089226, -0.3712484392070565797 ) ) ;
#14731 = EDGE_CURVE ( 'NONE', #6904, #541, #13766, .T. ) ;
#14732 = VECTOR ( 'NONE', #14424, 1000.000000000000000 ) ;
#14733 = EDGE_CURVE ( 'NONE', #7541, #10091, #15135, .T. ) ;
#14734 = FACE_BOUND ( 'NONE', #10569, .T. ) ;
#14735 = CIRCLE ( 'NONE', #7084, 2.750000000000002665 ) ;
#14736 = CARTESIAN_POINT ( 'NONE',  ( 3.783699349552338997, -3.968750000000262013, 0.7536532579988950431 ) ) ;
#14737 = CARTESIAN_POINT ( 'NONE',  ( -16.75000000000000000, -0.2038245569916330158, 23.22168783648699986 ) ) ;
#14738 = DIRECTION ( 'NONE',  ( 0.000000000000000000, 0.000000000000000000, 1.000000000000000000 ) ) ;
#14739 = DIRECTION ( 'NONE',  ( 0.000000000000000000, 0.000000000000000000, -1.000000000000000000 ) ) ;
#14740 = CARTESIAN_POINT ( 'NONE',  ( -3.980019242547642833, -0.5625000000000109912, 1.650257999534034514 ) ) ;
#14741 = CARTESIAN_POINT ( 'NONE',  ( -54.81638362644100226, 97.99516924618178848, -150.4984795835770228 ) ) ;
#14742 = DIRECTION ( 'NONE',  ( 0.000000000000000000, 0.000000000000000000, 1.000000000000000000 ) ) ;
#14743 = PRODUCT_DEFINITION_SHAPE ( 'NONE', 'NONE',  #5538 ) ;
#14744 = CARTESIAN_POINT ( 'NONE',  ( 3.584540577507836603E-16, 9.015594676761164550, 0.000000000000000000 ) ) ;
#14745 = ADVANCED_FACE ( 'NONE', ( #10175 ), #12831, .F. ) ;
#14746 = VERTEX_POINT ( 'NONE', #1027 ) ;
#14747 = CARTESIAN_POINT ( 'NONE',  ( 68.41329019055577021, 5.000000000000000000, 91.50956111919110469 ) ) ;
#14748 = ORIENTED_EDGE ( 'NONE', *, *, #13416, .F. ) ;
#14749 = VECTOR ( 'NONE', #2525, 1000.000000000000000 ) ;
#14750 = VERTEX_POINT ( 'NONE', #3138 ) ;
#14751 = VERTEX_POINT ( 'NONE', #1969 ) ;
#14752 = CIRCLE ( 'NONE', #10534, 3.299999999999473577 ) ;
#14753 = PRODUCT_DEFINITION_CONTEXT ( 'detailed design', #9313, 'design' ) ;
#14754 = EDGE_CURVE ( 'NONE', #14499, #1968, #10338, .T. ) ;
#14755 = CARTESIAN_POINT ( 'NONE',  ( -69.77438362644001302, 71.67411849586700612, -80.44847958357698303 ) ) ;
#14756 = CARTESIAN_POINT ( 'NONE',  ( 3.124039007639229037, -5.631874999999973319, -0.9468071286117496488 ) ) ;
#14757 = EDGE_CURVE ( 'NONE', #14091, #1421, #8014, .T. ) ;
#14758 = EDGE_CURVE ( 'NONE', #2834, #10983, #3012, .T. ) ;
#14759 = FACE_OUTER_BOUND ( 'NONE', #15178, .T. ) ;
#14760 = DIRECTION ( 'NONE',  ( 0.3469356515732570645, 0.9378889346118971515, 0.000000000000000000 ) ) ;
#14761 = LINE ( 'NONE', #6337, #9309 ) ;
#14762 = AXIS2_PLACEMENT_3D ( 'NONE', #24, #2587, #7335 ) ;
#14763 = CARTESIAN_POINT ( 'NONE',  ( 22.58164641901421632, -12.00000029085423670, -11.73358795631401463 ) ) ;
#14764 = DIRECTION ( 'NONE',  ( 0.000000000000000000, 0.000000000000000000, 1.000000000000000000 ) ) ;
#14765 = CIRCLE ( 'NONE', #11804, 4.249999999999996447 ) ;
#14766 = CARTESIAN_POINT ( 'NONE',  ( 3.333123593314366140, -4.616249999999967990, -0.6642911394208504960 ) ) ;
#14767 = EDGE_LOOP ( 'NONE', ( #1204, #13529, #8595, #1530 ) ) ;
#14768 = LINE ( 'NONE', #13686, #4898 ) ;
#14769 = CIRCLE ( 'NONE', #4624, 1.785937500000001066 ) ;
#14770 = ORIENTED_EDGE ( 'NONE', *, *, #119, .T. ) ;
#14771 = AXIS2_PLACEMENT_3D ( 'NONE', #11579, #7932, #7790 ) ;
#14772 = CARTESIAN_POINT ( 'NONE',  ( -2.852666340614860463, -2.624999999999946265, 2.854740429567705018 ) ) ;
#14773 = ORIENTED_EDGE ( 'NONE', *, *, #13897, .T. ) ;
#14774 = VECTOR ( 'NONE', #5850, 1000.000000000000000 ) ;
#14775 = FACE_OUTER_BOUND ( 'NONE', #5387, .T. ) ;
#14776 = PLANE ( 'NONE',  #9783 ) ;
#14777 = FACE_OUTER_BOUND ( 'NONE', #1931, .T. ) ;
#14778 = VECTOR ( 'NONE', #6982, 1000.000000000000000 ) ;
#14779 = LINE ( 'NONE', #15075, #1961 ) ;
#14780 = CARTESIAN_POINT ( 'NONE',  ( -2.193587568837934931, 1.881091898551119135, 4.500000000000000888 ) ) ;
#14781 = DIRECTION ( 'NONE',  ( 1.000000000000000000, 0.000000000000000000, 0.000000000000000000 ) ) ;
#14782 = CARTESIAN_POINT ( 'NONE',  ( -72.92551479769302603, 97.86074886511958937, -93.49847958357699440 ) ) ;
#14783 = FACE_OUTER_BOUND ( 'NONE', #13428, .T. ) ;
#14784 = VERTEX_POINT ( 'NONE', #12672 ) ;
#14785 = ORIENTED_EDGE ( 'NONE', *, *, #4110, .T. ) ;
#14786 = CARTESIAN_POINT ( 'NONE',  ( -3.224082633657789465, -0.9912500000000042943, -2.155484159616802398 ) ) ;
#14787 = VERTEX_POINT ( 'NONE', #7873 ) ;
#14788 = CIRCLE ( 'NONE', #8108, 0.5999999999999998668 ) ;
#14789 = DIRECTION ( 'NONE',  ( 0.000000000000000000, 0.000000000000000000, 1.000000000000000000 ) ) ;
#14790 = CARTESIAN_POINT ( 'NONE',  ( 23.25000000000000000, -10.00000000000000000, -27.00000000000000000 ) ) ;
#14791 = DIRECTION ( 'NONE',  ( 1.000000000000000000, 0.000000000000000000, 0.000000000000000000 ) ) ;
#14792 = CARTESIAN_POINT ( 'NONE',  ( -55.52438362644000591, 99.17411849586700612, -86.49847958357699440 ) ) ;
#14793 = CARTESIAN_POINT ( 'NONE',  ( -35.27438362644000591, 60.67411849586700612, -67.49847958357700861 ) ) ;
#14794 = EDGE_CURVE ( 'NONE', #10105, #11586, #6981, .T. ) ;
#14795 = PLANE ( 'NONE',  #14159 ) ;
#14796 = AXIS2_PLACEMENT_3D ( 'NONE', #6782, #10329, #7933 ) ;
#14797 = ORIENTED_EDGE ( 'NONE', *, *, #4403, .F. ) ;
#14798 = DIRECTION ( 'NONE',  ( 0.000000000000000000, 0.000000000000000000, -1.000000000000000000 ) ) ;
#14799 = EDGE_CURVE ( 'NONE', #13889, #4585, #274, .T. ) ;
#14800 = ORIENTED_EDGE ( 'NONE', *, *, #11955, .F. ) ;
#14801 = EDGE_LOOP ( 'NONE', ( #7921, #10447, #13750, #13073 ) ) ;
#14802 = ORIENTED_EDGE ( 'NONE', *, *, #14053, .T. ) ;
#14803 = ORIENTED_EDGE ( 'NONE', *, *, #6424, .T. ) ;
#14804 = EDGE_LOOP ( 'NONE', ( #341, #7268, #13602, #5841 ) ) ;
#14805 = DIRECTION ( 'NONE',  ( 0.000000000000000000, 0.000000000000000000, 1.000000000000000000 ) ) ;
#14806 = CARTESIAN_POINT ( 'NONE',  ( 3.647531283552059023, -2.600625000000050591, -0.3606074429803771131 ) ) ;
#14807 = VECTOR ( 'NONE', #13190, 1000.000000000000000 ) ;
#14808 = CARTESIAN_POINT ( 'NONE',  ( -86.77438362644100778, 99.17411849586700612, -182.2484795835770228 ) ) ;
#14809 = CARTESIAN_POINT ( 'NONE',  ( 2.991150664073139342, -3.890625000000195399, 2.452944570972435567 ) ) ;
#14810 = CARTESIAN_POINT ( 'NONE',  ( -84.73238362643999722, 63.99516924618178848, -147.9984795835769944 ) ) ;
#14811 = DIRECTION ( 'NONE',  ( -1.000000000000000000, 0.000000000000000000, 0.000000000000000000 ) ) ;
#14812 = DIRECTION ( 'NONE',  ( 0.000000000000000000, 0.000000000000000000, -1.000000000000000000 ) ) ;
#14813 = CARTESIAN_POINT ( 'NONE',  ( -1.643569066580401916, -0.6875000000000854872, 3.964934652274553439 ) ) ;
#14814 = CARTESIAN_POINT ( 'NONE',  ( -86.77438362643999881, 67.53201699523744139, -147.9984795835769944 ) ) ;
#14815 = ADVANCED_FACE ( 'NONE', ( #6867 ), #2046, .F. ) ;
#14816 = CARTESIAN_POINT ( 'NONE',  ( -73.01311196519618818, 67.29799558322736175, -83.44847958357698303 ) ) ;
#14817 = CARTESIAN_POINT ( 'NONE',  ( 17.18164641901421419, -2.908542394189813650E-07, 0.2664120436859911956 ) ) ;
#14818 = ORIENTED_EDGE ( 'NONE', *, *, #15018, .F. ) ;
#14819 = CARTESIAN_POINT ( 'NONE',  ( -86.77438362643999881, 65.17411849586700612, -147.9984795835769944 ) ) ;
#14820 = EDGE_CURVE ( 'NONE', #6505, #12175, #3599, .T. ) ;
#14821 = ORIENTED_EDGE ( 'NONE', *, *, #5539, .T. ) ;
#14822 = AXIS2_PLACEMENT_3D ( 'NONE', #7754, #13936, #2150 ) ;
#14823 = ORIENTED_EDGE ( 'NONE', *, *, #3081, .F. ) ;
#14824 = ORIENTED_EDGE ( 'NONE', *, *, #595, .F. ) ;
#14825 = CARTESIAN_POINT ( 'NONE',  ( -69.77438362644001302, 92.67411849586700612, -80.44847958357698303 ) ) ;
#14826 = CARTESIAN_POINT ( 'NONE',  ( -0.3227798623957894297, -5.319375000000161613, 3.289865787063878333 ) ) ;
#14827 = EDGE_CURVE ( 'NONE', #8472, #14103, #13220, .T. ) ;
#14828 = CARTESIAN_POINT ( 'NONE',  ( 4.573385150445044900, -19.31989681812820692, 0.000000000000000000 ) ) ;
#14829 = ADVANCED_FACE ( 'NONE', ( #6103 ), #2263, .T. ) ;
#14830 = LINE ( 'NONE', #4214, #4268 ) ;
#14831 = CARTESIAN_POINT ( 'NONE',  ( -59.02799568714584666, 103.6741184958669919, -73.34256232478206528 ) ) ;
#14832 = CIRCLE ( 'NONE', #4193, 2.042000000000002036 ) ;
#14833 = DIRECTION ( 'NONE',  ( 1.000000000000000000, 0.000000000000000000, -0.000000000000000000 ) ) ;
#14834 = CARTESIAN_POINT ( 'NONE',  ( 1.824979221380550021, -0.4995676945082544451, 3.571726915116150813 ) ) ;
#14835 = EDGE_CURVE ( 'NONE', #6571, #9068, #9945, .T. ) ;
#14836 = CARTESIAN_POINT ( 'NONE',  ( -2.931404194366994176, 4.650702586819535966, 0.000000000000000000 ) ) ;
#14837 = ORIENTED_EDGE ( 'NONE', *, *, #12568, .F. ) ;
#14838 = DIRECTION ( 'NONE',  ( 0.000000000000000000, 0.000000000000000000, 1.000000000000000000 ) ) ;
#14839 = VERTEX_POINT ( 'NONE', #7179 ) ;
#14840 = ADVANCED_FACE ( 'NONE', ( #3513 ), #9634, .F. ) ;
#14841 = VERTEX_POINT ( 'NONE', #6021 ) ;
#14842 = CARTESIAN_POINT ( 'NONE',  ( 2.623679764461153141, -1.859375000000051070, 3.198691315062023310 ) ) ;
#14843 = VERTEX_POINT ( 'NONE', #5947 ) ;
#14844 = DIRECTION ( 'NONE',  ( -1.000000000000000000, 0.000000000000000000, 0.000000000000000000 ) ) ;
#14845 = CARTESIAN_POINT ( 'NONE',  ( 37.35543536254874653, -19.31989681812820692, 6.000000000000000000 ) ) ;
#14846 = DIRECTION ( 'NONE',  ( 0.000000000000000000, 0.000000000000000000, -1.000000000000000000 ) ) ;
#14847 = EDGE_CURVE ( 'NONE', #4158, #4974, #7728, .T. ) ;
#14848 = FACE_OUTER_BOUND ( 'NONE', #8469, .T. ) ;
#14849 = DIRECTION ( 'NONE',  ( 0.000000000000000000, 0.000000000000000000, 1.000000000000000000 ) ) ;
#14850 = FACE_OUTER_BOUND ( 'NONE', #13406, .T. ) ;
#14851 = CARTESIAN_POINT ( 'NONE',  ( -86.77438362644001302, 99.17411849586700612, -86.49847958357699440 ) ) ;
#14852 = DIRECTION ( 'NONE',  ( 1.000000000000000000, 0.000000000000000000, 0.000000000000000000 ) ) ;
#14853 = DIRECTION ( 'NONE',  ( 1.000000000000000000, 0.000000000000000000, 0.000000000000000000 ) ) ;
#14854 = ORIENTED_EDGE ( 'NONE', *, *, #4980, .F. ) ;
#14855 = DIRECTION ( 'NONE',  ( 0.000000000000000000, 0.000000000000000000, 1.000000000000000000 ) ) ;
#14856 = CARTESIAN_POINT ( 'NONE',  ( 3.503209385669603382, -1.647500000000019948, -1.450007420588574680 ) ) ;
#14857 = ORIENTED_EDGE ( 'NONE', *, *, #2703, .T. ) ;
#14858 = DIRECTION ( 'NONE',  ( 0.000000000000000000, 0.000000000000000000, -1.000000000000000000 ) ) ;
#14859 = FACE_OUTER_BOUND ( 'NONE', #13471, .T. ) ;
#14860 = CARTESIAN_POINT ( 'NONE',  ( -1.543400882162985400E-14, 7.839999999999998082, 5.619086434621074034E-29 ) ) ;
#14861 = PRESENTATION_STYLE_ASSIGNMENT (( #12332 ) ) ;
#14862 = DIRECTION ( 'NONE',  ( 0.000000000000000000, 0.000000000000000000, -1.000000000000000000 ) ) ;
#14863 = DIRECTION ( 'NONE',  ( 0.000000000000000000, 0.000000000000000000, 1.000000000000000000 ) ) ;
#14864 = ORIENTED_EDGE ( 'NONE', *, *, #5180, .T. ) ;
#14865 = DIRECTION ( 'NONE',  ( 0.000000000000000000, 0.000000000000000000, -1.000000000000000000 ) ) ;
#14866 = ORIENTED_EDGE ( 'NONE', *, *, #5955, .T. ) ;
#14867 = EDGE_LOOP ( 'NONE', ( #8231, #970, #6443, #1151 ) ) ;
#14868 = VERTEX_POINT ( 'NONE', #12057 ) ;
#14869 = ORIENTED_EDGE ( 'NONE', *, *, #2177, .F. ) ;
#14870 = VERTEX_POINT ( 'NONE', #2578 ) ;
#14871 = AXIS2_PLACEMENT_3D ( 'NONE', #5324, #437, #10040 ) ;
#14872 = FACE_OUTER_BOUND ( 'NONE', #1756, .T. ) ;
#14873 = CARTESIAN_POINT ( 'NONE',  ( 1.916065064279496746E-15, 7.362499999999997158, 0.000000000000000000 ) ) ;
#14874 = VECTOR ( 'NONE', #12776, 1000.000000000000000 ) ;
#14875 = CARTESIAN_POINT ( 'NONE',  ( 14.25000000000000000, -2.500000000000000000, -21.77831216351300014 ) ) ;
#14876 = CARTESIAN_POINT ( 'NONE',  ( 4.118464008547413790, -2.000000000000003109, 0.001090570402295849319 ) ) ;
#14877 = CARTESIAN_POINT ( 'NONE',  ( 2.598076211353314235, 0.1227504548087474667, -4.499999999999999112 ) ) ;
#14878 = CARTESIAN_POINT ( 'NONE',  ( -79.11147769456633227, 68.38713492810558137, -83.44847958357698303 ) ) ;
#14879 = DIRECTION ( 'NONE',  ( 0.000000000000000000, 1.000000000000000000, 0.000000000000000000 ) ) ;
#14880 = CARTESIAN_POINT ( 'NONE',  ( -4.125408418587476866, -0.5468750000000269784, 1.250226324283678192 ) ) ;
#14881 = DIRECTION ( 'NONE',  ( 0.000000000000000000, 0.000000000000000000, 1.000000000000000000 ) ) ;
#14882 = FACE_OUTER_BOUND ( 'NONE', #3360, .T. ) ;
#14883 = CARTESIAN_POINT ( 'NONE',  ( -16.33757311576526305, -0.3152598339554808504, -21.54019739087904384 ) ) ;
#14884 = AXIS2_PLACEMENT_3D ( 'NONE', #3910, #8938, #333 ) ;
#14885 = ORIENTED_EDGE ( 'NONE', *, *, #14409, .T. ) ;
#14886 = CARTESIAN_POINT ( 'NONE',  ( -69.77438362644001302, 99.17411849586700612, -81.84847958357698872 ) ) ;
#14887 = EDGE_LOOP ( 'NONE', ( #3477, #8914, #11991, #9255, #1835 ) ) ;
#14888 = EDGE_LOOP ( 'NONE', ( #11701, #3720, #4451, #7658 ) ) ;
#14889 = ORIENTED_EDGE ( 'NONE', *, *, #1274, .F. ) ;
#14890 = B_SPLINE_CURVE_WITH_KNOTS ( 'NONE', 3,
 ( #6091, #10802, #13067, #10637, #10882, #12045 ),
 .UNSPECIFIED., .F., .F.,
 ( 4, 2, 4 ),
 ( 0.0002380763768113913770, 0.7291065797294570272, 1.457975083082102774 ),
 .UNSPECIFIED. ) ;
#14891 = DIRECTION ( 'NONE',  ( 0.000000000000000000, 0.000000000000000000, 1.000000000000000000 ) ) ;
#14892 = PRODUCT_DEFINITION ( 'UNKNOWN', '', #7193, #12433 ) ;
#14893 = EDGE_CURVE ( 'NONE', #12927, #11166, #13132, .T. ) ;
#14894 = CARTESIAN_POINT ( 'NONE',  ( -3.069066067673428932, -4.006874999999906706, -1.638984897852511891 ) ) ;
#14895 = AXIS2_PLACEMENT_3D ( 'NONE', #3202, #716, #9315 ) ;
#14896 = LINE ( 'NONE', #4285, #159 ) ;
#14897 = DIRECTION ( 'NONE',  ( 0.000000000000000000, 0.000000000000000000, 1.000000000000000000 ) ) ;
#14898 = CARTESIAN_POINT ( 'NONE',  ( 5.196152422706626695, 1.678847577293385296, -1.115338501812287204E-15 ) ) ;
#14899 = DIRECTION ( 'NONE',  ( 0.000000000000000000, 0.000000000000000000, 1.000000000000000000 ) ) ;
#14900 = CARTESIAN_POINT ( 'NONE',  ( -4.193021748915730207, -0.4995676945082699327, 0.9078562877249845009 ) ) ;
#14901 = FACE_OUTER_BOUND ( 'NONE', #5442, .T. ) ;
#14902 = VECTOR ( 'NONE', #10063, 1000.000000000000000 ) ;
#14903 = DIRECTION ( 'NONE',  ( 0.4999999999999827360, 0.000000000000000000, -0.8660254037844485886 ) ) ;
#14904 = ORIENTED_EDGE ( 'NONE', *, *, #4615, .T. ) ;
#14905 = CARTESIAN_POINT ( 'NONE',  ( -52.77438362644000591, 65.17411849586700612, -86.49847958357699440 ) ) ;
#14906 = VERTEX_POINT ( 'NONE', #1425 ) ;
#14907 = COLOUR_RGB ( '', 0.08235294, 0.09019608, 0.10196078) ;
#14908 = EDGE_CURVE ( 'NONE', #953, #9311, #7961, .T. ) ;
#14909 = CARTESIAN_POINT ( 'NONE',  ( -77.89938362643999881, 82.17411849586700612, -79.49847958357700861 ) ) ;
#14910 = VERTEX_POINT ( 'NONE', #12903 ) ;
#14911 = CARTESIAN_POINT ( 'NONE',  ( -2.727692609523614475, -0.6406250000000671685, 3.321895092029963248 ) ) ;
#14912 = ORIENTED_EDGE ( 'NONE', *, *, #2817, .T. ) ;
#14913 = CIRCLE ( 'NONE', #1552, 2.699999999999993960 ) ;
#14914 = ADVANCED_FACE ( 'NONE', ( #2498 ), #15218, .F. ) ;
#14915 = CARTESIAN_POINT ( 'NONE',  ( -2.759584380001296910, -3.624213562373039377, 2.761600069345273134 ) ) ;
#14916 = DIRECTION ( 'NONE',  ( 0.000000000000000000, 0.000000000000000000, 1.000000000000000000 ) ) ;
#14917 = EDGE_CURVE ( 'NONE', #8137, #13129, #14156, .T. ) ;
#14918 = DIRECTION ( 'NONE',  ( 1.000000000000000000, 0.000000000000000000, 0.000000000000000000 ) ) ;
#14919 =( GEOMETRIC_REPRESENTATION_CONTEXT ( 3 ) GLOBAL_UNCERTAINTY_ASSIGNED_CONTEXT ( ( #2970 ) ) GLOBAL_UNIT_ASSIGNED_CONTEXT ( ( #10862, #10782, #146 ) ) REPRESENTATION_CONTEXT ( 'NONE', 'WORKASPACE' ) );
#14920 = ADVANCED_FACE ( 'NONE', ( #4926, #10572 ), #6474, .T. ) ;
#14921 = CARTESIAN_POINT ( 'NONE',  ( -90.52438362644100778, 99.17411849586700612, -150.4984795835770228 ) ) ;
#14922 = CARTESIAN_POINT ( 'NONE',  ( 21.98164641901421135, -2.908542394189813650E-07, 0.2664120436859911956 ) ) ;
#14923 = FACE_OUTER_BOUND ( 'NONE', #10775, .T. ) ;
#14924 = CARTESIAN_POINT ( 'NONE',  ( -15.50000000000000000, -1.037157890325000054, -22.50000000000000000 ) ) ;
#14925 = DIRECTION ( 'NONE',  ( -0.000000000000000000, -0.000000000000000000, 1.000000000000000000 ) ) ;
#14926 = AXIS2_PLACEMENT_3D ( 'NONE', #10536, #2008, #12798 ) ;
#14927 = VECTOR ( 'NONE', #10087, 1000.000000000000000 ) ;
#14928 = CARTESIAN_POINT ( 'NONE',  ( -77.89938362643999881, 82.17411849586700612, -93.49847958357699440 ) ) ;
#14929 = ADVANCED_FACE ( 'NONE', ( #10892 ), #8801, .T. ) ;
#14930 = ORIENTED_EDGE ( 'NONE', *, *, #8298, .T. ) ;
#14931 = CARTESIAN_POINT ( 'NONE',  ( -2.896649075160178111, -1.975624999999826548, -2.378478989283399958 ) ) ;
#14932 = VERTEX_POINT ( 'NONE', #14444 ) ;
#14933 = EDGE_CURVE ( 'NONE', #9845, #4841, #9185, .T. ) ;
#14934 = VECTOR ( 'NONE', #3216, 999.9999999999998863 ) ;
#14935 = DIRECTION ( 'NONE',  ( -1.000000000000000000, 0.000000000000000000, 0.000000000000000000 ) ) ;
#14936 = CARTESIAN_POINT ( 'NONE',  ( 57.41329019055577021, 5.000000000000001776, 133.4783111191910621 ) ) ;
#14937 = CARTESIAN_POINT ( 'NONE',  ( 17.12895037488186389, -3.654606557864051197, 0.2687305842673423095 ) ) ;
#14938 = VECTOR ( 'NONE', #2171, 1000.000000000000000 ) ;
#14939 = DIRECTION ( 'NONE',  ( 0.7071067811865474617, -0.000000000000000000, 0.7071067811865474617 ) ) ;
#14940 = CARTESIAN_POINT ( 'NONE',  ( -15.50000000000000000, -1.037157890325000054, -22.50000000000000000 ) ) ;
#14941 = CARTESIAN_POINT ( 'NONE',  ( 15.50000000000000000, -2.500000000000000000, -23.94337567297399971 ) ) ;
#14942 = CARTESIAN_POINT ( 'NONE',  ( 15.50000000000000000, -0.1999999999999999556, -22.50000000000000000 ) ) ;
#14943 = VERTEX_POINT ( 'NONE', #13221 ) ;
#14944 = DIRECTION ( 'NONE',  ( 0.000000000000000000, 0.000000000000000000, 1.000000000000000000 ) ) ;
#14945 = VECTOR ( 'NONE', #10284, 1000.000000000000000 ) ;
#14946 = VERTEX_POINT ( 'NONE', #12058 ) ;
#14947 = ORIENTED_EDGE ( 'NONE', *, *, #13959, .T. ) ;
#14948 = CARTESIAN_POINT ( 'NONE',  ( 3.124039007639229482, -5.631874999999973319, -0.9468071286117497598 ) ) ;
#14949 = EDGE_LOOP ( 'NONE', ( #6849, #10871, #10960, #9567 ) ) ;
#14950 = ORIENTED_EDGE ( 'NONE', *, *, #15004, .T. ) ;
#14951 = VERTEX_POINT ( 'NONE', #1428 ) ;
#14952 = CARTESIAN_POINT ( 'NONE',  ( 1.704156345177410881, -5.827338562373107322, 3.185422574234377358 ) ) ;
#14953 = CARTESIAN_POINT ( 'NONE',  ( 3.459076575081923899, -0.6631250000000769029, -1.847748348019847109 ) ) ;
#14954 = FACE_OUTER_BOUND ( 'NONE', #13667, .T. ) ;
#14955 = CARTESIAN_POINT ( 'NONE',  ( -1.185531852251327400, -2.296875000000050182, -3.903075577084617720 ) ) ;
#14956 = AXIS2_PLACEMENT_3D ( 'NONE', #7678, #8520, #5035 ) ;
#14957 = CARTESIAN_POINT ( 'NONE',  ( -86.77438362644001302, 65.17411849586700612, -152.4984795835769944 ) ) ;
#14958 = VECTOR ( 'NONE', #12779, 1000.000000000000000 ) ;
#14959 = DIRECTION ( 'NONE',  ( -0.000000000000000000, -1.000000000000000000, -0.000000000000000000 ) ) ;
#14960 = CARTESIAN_POINT ( 'NONE',  ( -86.77438362644100778, 101.5320169952374414, -147.9984795835769944 ) ) ;
#14961 = LINE ( 'NONE', #4353, #9952 ) ;
#14962 = DIRECTION ( 'NONE',  ( -1.000000000000000000, 0.000000000000000000, 0.000000000000000000 ) ) ;
#14963 = CARTESIAN_POINT ( 'NONE',  ( -73.51240544634549678, 65.59017466835992138, -81.84847958357697451 ) ) ;
#14964 = FACE_OUTER_BOUND ( 'NONE', #13580, .T. ) ;
#14965 = ORIENTED_EDGE ( 'NONE', *, *, #1576, .F. ) ;
#14966 = CARTESIAN_POINT ( 'NONE',  ( -75.01311196519617397, 67.29799558322736175, -81.84847958357697451 ) ) ;
#14967 = ORIENTED_EDGE ( 'NONE', *, *, #12386, .F. ) ;
#14968 = VERTEX_POINT ( 'NONE', #6184 ) ;
#14969 = ORIENTED_EDGE ( 'NONE', *, *, #5754, .T. ) ;
#14970 = EDGE_CURVE ( 'NONE', #913, #12871, #5242, .T. ) ;
#14971 = CARTESIAN_POINT ( 'NONE',  ( 16.75000000000000000, -2.500000000000000000, -21.77831216351300014 ) ) ;
#14972 = CIRCLE ( 'NONE', #9525, 1.785937500000001066 ) ;
#14973 = CARTESIAN_POINT ( 'NONE',  ( -2.894177851434075244, -3.991249999999941789, -1.934899151906914305 ) ) ;
#14974 = DIRECTION ( 'NONE',  ( 0.000000000000000000, -4.336808689942017736E-16, 1.000000000000000000 ) ) ;
#14975 = LINE ( 'NONE', #12891, #13922 ) ;
#14976 = CARTESIAN_POINT ( 'NONE',  ( -46.58670980944423690, 5.000000000000000000, 137.5095611191910621 ) ) ;
#14977 = CARTESIAN_POINT ( 'NONE',  ( -68.41221392010794489, 74.17411849586699191, -58.99847958357693756 ) ) ;
#14978 = CARTESIAN_POINT ( 'NONE',  ( 3.141122330734205104, -0.4995676945082517251, 2.389792696361102919 ) ) ;
#14979 = CARTESIAN_POINT ( 'NONE',  ( -85.75338362644100698, 100.9425423703948326, -147.9984795835769944 ) ) ;
#14980 = CIRCLE ( 'NONE', #14007, 8.050000000000000711 ) ;
#14981 = EDGE_LOOP ( 'NONE', ( #1146, #15193, #15251, #8053, #10214, #4647 ) ) ;
#14982 = AXIS2_PLACEMENT_3D ( 'NONE', #10673, #2151, #5812 ) ;
#14983 = CARTESIAN_POINT ( 'NONE',  ( 2.919796888921922573, -5.104126807837104707, -2.256669152708658643 ) ) ;
#14984 = EDGE_CURVE ( 'NONE', #11838, #11568, #15298, .T. ) ;
#14985 = ORIENTED_EDGE ( 'NONE', *, *, #9140, .T. ) ;
#14986 = ORIENTED_EDGE ( 'NONE', *, *, #8602, .T. ) ;
#14987 = EDGE_CURVE ( 'NONE', #3597, #12145, #636, .T. ) ;
#14988 = CARTESIAN_POINT ( 'NONE',  ( 2.013502677559834808, -0.8281249999998109290, 3.769415173278118480 ) ) ;
#14989 = VERTEX_POINT ( 'NONE', #5225 ) ;
#14990 = AXIS2_PLACEMENT_3D ( 'NONE', #3820, #11965, #8546 ) ;
#14991 = CARTESIAN_POINT ( 'NONE',  ( -0.4017660263608561211, -2.264838562373181041, -4.064082169119537902 ) ) ;
#14992 = CIRCLE ( 'NONE', #1390, 1.250000000000001110 ) ;
#14993 = AXIS2_PLACEMENT_3D ( 'NONE', #5250, #3153, #6433 ) ;
#14994 = DIRECTION ( 'NONE',  ( 0.8660254037844387076, 0.4999999999999998890, 0.000000000000000000 ) ) ;
#14995 = DIRECTION ( 'NONE',  ( 1.000000000000000000, 0.000000000000000000, 0.000000000000000000 ) ) ;
#14996 = CARTESIAN_POINT ( 'NONE',  ( -35.58670980944424400, 5.000000000000001776, 97.50956111919106206 ) ) ;
#14997 = CARTESIAN_POINT ( 'NONE',  ( -52.77438362644000591, 65.17411849586700612, -152.4984795835769944 ) ) ;
#14998 = AXIS2_PLACEMENT_3D ( 'NONE', #12320, #1685, #12088 ) ;
#14999 = CARTESIAN_POINT ( 'NONE',  ( 15.50000000000000000, -2.500000000000000000, 23.94337567297399971 ) ) ;
#15000 = EDGE_CURVE ( 'NONE', #7286, #3237, #11675, .T. ) ;
#15001 = VECTOR ( 'NONE', #14288, 1000.000000000000114 ) ;
#15002 = AXIS2_PLACEMENT_3D ( 'NONE', #9740, #7591, #8428 ) ;
#15003 = ORIENTED_EDGE ( 'NONE', *, *, #4556, .T. ) ;
#15004 = EDGE_CURVE ( 'NONE', #11427, #7228, #4141, .T. ) ;
#15005 = DIRECTION ( 'NONE',  ( 0.000000000000000000, 0.000000000000000000, -1.000000000000000000 ) ) ;
#15006 = CARTESIAN_POINT ( 'NONE',  ( -2.210630411551929519, -0.2412499999998789502, 3.306558829207998595 ) ) ;
#15007 = ORIENTED_EDGE ( 'NONE', *, *, #2411, .F. ) ;
#15008 = CIRCLE ( 'NONE', #15266, 1.785937500000001066 ) ;
#15009 = CARTESIAN_POINT ( 'NONE',  ( 2.605880849243368491, -2.459999999999848086, 2.603962797083386072 ) ) ;
#15010 = DIRECTION ( 'NONE',  ( 0.000000000000000000, -0.000000000000000000, 1.000000000000000000 ) ) ;
#15011 = VECTOR ( 'NONE', #10856, 1000.000000000000000 ) ;
#15012 = EDGE_CURVE ( 'NONE', #14573, #8182, #9940, .T. ) ;
#15013 = DIRECTION ( 'NONE',  ( 0.000000000000000000, -4.130293990420970006E-17, 1.000000000000000000 ) ) ;
#15014 = DIRECTION ( 'NONE',  ( 1.000000000000000000, 0.000000000000000000, 0.000000000000000000 ) ) ;
#15015 = PLANE ( 'NONE',  #10873 ) ;
#15016 = FILL_AREA_STYLE ('',( #12936 ) ) ;
#15017 = CYLINDRICAL_SURFACE ( 'NONE', #12774, 8.000000000000007105 ) ;
#15018 = EDGE_CURVE ( 'NONE', #2765, #14932, #4007, .T. ) ;
#15019 = DIRECTION ( 'NONE',  ( -1.000000000000000000, 0.000000000000000000, 0.000000000000000000 ) ) ;
#15020 = ORIENTED_EDGE ( 'NONE', *, *, #13056, .F. ) ;
#15021 = DIRECTION ( 'NONE',  ( 1.000000000000000000, 0.000000000000000000, 0.000000000000000000 ) ) ;
#15022 = AXIS2_PLACEMENT_3D ( 'NONE', #1735, #5551, #5405 ) ;
#15023 = VERTEX_POINT ( 'NONE', #5391 ) ;
#15024 = ADVANCED_FACE ( 'NONE', ( #414 ), #11119, .F. ) ;
#15025 = VECTOR ( 'NONE', #496, 1000.000000000000000 ) ;
#15026 = ORIENTED_EDGE ( 'NONE', *, *, #2088, .F. ) ;
#15027 = ADVANCED_FACE ( 'NONE', ( #13534 ), #11183, .F. ) ;
#15028 = EDGE_LOOP ( 'NONE', ( #7242, #7374 ) ) ;
#15029 = ORIENTED_EDGE ( 'NONE', *, *, #13490, .F. ) ;
#15030 = ORIENTED_EDGE ( 'NONE', *, *, #11251, .T. ) ;
#15031 = CARTESIAN_POINT ( 'NONE',  ( -3.215696830464670697, -5.577338562373121533, 1.717757276957577073 ) ) ;
#15032 = CARTESIAN_POINT ( 'NONE',  ( -2.441443777772203561, -1.225625000000065912, 2.973322847374053612 ) ) ;
#15033 = SURFACE_SIDE_STYLE ('',( #4422 ) ) ;
#15034 = CARTESIAN_POINT ( 'NONE',  ( 3.303237764219515427, -3.093750000000110578, -2.208893390251179589 ) ) ;
#15035 = CARTESIAN_POINT ( 'NONE',  ( -69.77438362644001302, 82.17411849586700612, -182.1969643934119745 ) ) ;
#15036 = CARTESIAN_POINT ( 'NONE',  ( -69.77438362644001302, 82.17411849586700612, -80.44847958357698303 ) ) ;
#15037 = AXIS2_PLACEMENT_3D ( 'NONE', #6540, #4200, #1714 ) ;
#15038 = CARTESIAN_POINT ( 'NONE',  ( 2.598076211353311127, 1.678847577293378190, 4.500000000000000000 ) ) ;
#15039 = CARTESIAN_POINT ( 'NONE',  ( -52.77438362643999881, 62.81621999649657084, -147.9984795835769944 ) ) ;
#15040 = CYLINDRICAL_SURFACE ( 'NONE', #6825, 3.499999999999999556 ) ;
#15041 = CARTESIAN_POINT ( 'NONE',  ( 16.54633693294649888, -0.2717122460102533998, -21.66072723692568402 ) ) ;
#15042 = LINE ( 'NONE', #6628, #13718 ) ;
#15043 = ORIENTED_EDGE ( 'NONE', *, *, #10855, .T. ) ;
#15044 = CARTESIAN_POINT ( 'NONE',  ( -2.779367716467973093, 7.159503395827459929E-16, 50.11303170532690388 ) ) ;
#15045 = ORIENTED_EDGE ( 'NONE', *, *, #805, .F. ) ;
#15046 = ORIENTED_EDGE ( 'NONE', *, *, #13535, .F. ) ;
#15047 = ORIENTED_EDGE ( 'NONE', *, *, #7879, .F. ) ;
#15048 = UNCERTAINTY_MEASURE_WITH_UNIT (LENGTH_MEASURE( 1.000000000000000082E-05 ), #3222, 'distance_accuracy_value', 'NONE');
#15049 = VECTOR ( 'NONE', #10696, 999.9999999999998863 ) ;
#15050 = CARTESIAN_POINT ( 'NONE',  ( 16.54633693294649532, -0.2717122460102548986, 23.33927276307431598 ) ) ;
#15051 = CARTESIAN_POINT ( 'NONE',  ( 3.009749400183384882, -4.506874999999939568, 1.609730366092098075 ) ) ;
#15052 = CARTESIAN_POINT ( 'NONE',  ( -84.73238362644100619, 100.3530677455522238, -147.9984795835769944 ) ) ;
#15053 = CARTESIAN_POINT ( 'NONE',  ( 2.598076211353308462, 2.375000000000006661, -4.499999999999999112 ) ) ;
#15054 = DIRECTION ( 'NONE',  ( 0.000000000000000000, 0.7547095802227716810, 0.6560590289905077199 ) ) ;
#15055 = CARTESIAN_POINT ( 'NONE',  ( -3.464101615137753054, -9.090049444189458401E-15, -2.999999999999999112 ) ) ;
#15056 = DIRECTION ( 'NONE',  ( 0.000000000000000000, 0.000000000000000000, 1.000000000000000000 ) ) ;
#15057 = PLANE ( 'NONE',  #4308 ) ;
#15058 = LINE ( 'NONE', #3353, #6575 ) ;
#15059 = AXIS2_PLACEMENT_3D ( 'NONE', #4250, #14017, #3229 ) ;
#15060 = ORIENTED_EDGE ( 'NONE', *, *, #12279, .T. ) ;
#15061 = LINE ( 'NONE', #1106, #4154 ) ;
#15062 = ORIENTED_EDGE ( 'NONE', *, *, #15306, .F. ) ;
#15063 = VERTEX_POINT ( 'NONE', #5159 ) ;
#15064 = PLANE ( 'NONE',  #11170 ) ;
#15065 = ORIENTED_EDGE ( 'NONE', *, *, #8100, .F. ) ;
#15066 = CARTESIAN_POINT ( 'NONE',  ( -0.4056240317154969355, -1.734374999999933831, 4.133709567805635920 ) ) ;
#15067 = VERTEX_POINT ( 'NONE', #1577 ) ;
#15068 = CARTESIAN_POINT ( 'NONE',  ( 1.148110318453624545, -3.202338562373148623, -3.789782819255727020 ) ) ;
#15069 = AXIS2_PLACEMENT_3D ( 'NONE', #7512, #13477, #443 ) ;
#15070 = CARTESIAN_POINT ( 'NONE',  ( -73.80978675135780520, 64.78624853950366003, -83.44847958357698303 ) ) ;
#15071 = EDGE_CURVE ( 'NONE', #5823, #4668, #10424, .T. ) ;
#15072 = DIRECTION ( 'NONE',  ( 0.000000000000000000, 0.000000000000000000, 1.000000000000000000 ) ) ;
#15073 = LINE ( 'NONE', #6875, #14934 ) ;
#15074 = ADVANCED_FACE ( 'NONE', ( #4061 ), #10182, .T. ) ;
#15075 = CARTESIAN_POINT ( 'NONE',  ( -16.75000000000000000, -2.500000000000000000, -23.22168783648699986 ) ) ;
#15076 = DIRECTION ( 'NONE',  ( 0.000000000000000000, 0.000000000000000000, 1.000000000000000000 ) ) ;
#15077 = DIRECTION ( 'NONE',  ( 0.000000000000000000, 1.000000000000000000, 0.000000000000000000 ) ) ;
#15078 = ORIENTED_EDGE ( 'NONE', *, *, #14604, .T. ) ;
#15079 = FILL_AREA_STYLE ('',( #9186 ) ) ;
#15080 = CARTESIAN_POINT ( 'NONE',  ( 0.3626941743317158018, -5.234374999999986677, -3.672738340478102437 ) ) ;
#15081 = ORIENTED_EDGE ( 'NONE', *, *, #3273, .F. ) ;
#15082 = EDGE_CURVE ( 'NONE', #5950, #10374, #3418, .T. ) ;
#15083 = CARTESIAN_POINT ( 'NONE',  ( 3.647531283552059023, -2.600625000000050591, -0.3606074429803771131 ) ) ;
#15084 = CARTESIAN_POINT ( 'NONE',  ( 68.41329019055577021, 5.000000000000000000, 135.5095611191910621 ) ) ;
#15085 = EDGE_CURVE ( 'NONE', #11568, #1588, #11438, .T. ) ;
#15086 = FACE_OUTER_BOUND ( 'NONE', #10320, .T. ) ;
#15087 = DIRECTION ( 'NONE',  ( 0.000000000000000000, 1.000000000000000000, 0.000000000000000000 ) ) ;
#15088 = DIRECTION ( 'NONE',  ( 1.000000000000000000, 0.000000000000000000, 0.000000000000000000 ) ) ;
#15089 = FACE_OUTER_BOUND ( 'NONE', #9612, .T. ) ;
#15090 = CARTESIAN_POINT ( 'NONE',  ( -14.25000000000000000, -2.500000000000000000, -23.22168783648699986 ) ) ;
#15091 = ORIENTED_EDGE ( 'NONE', *, *, #5287, .T. ) ;
#15092 = DIRECTION ( 'NONE',  ( 1.000000000000000000, 0.000000000000000000, 0.000000000000000000 ) ) ;
#15093 = ORIENTED_EDGE ( 'NONE', *, *, #8187, .T. ) ;
#15094 = EDGE_CURVE ( 'NONE', #10111, #384, #12133, .T. ) ;
#15095 = ORIENTED_EDGE ( 'NONE', *, *, #1356, .F. ) ;
#15096 = ORIENTED_EDGE ( 'NONE', *, *, #12718, .T. ) ;
#15097 = EDGE_CURVE ( 'NONE', #11360, #858, #1502, .T. ) ;
#15098 = ORIENTED_EDGE ( 'NONE', *, *, #13156, .F. ) ;
#15099 = ORIENTED_EDGE ( 'NONE', *, *, #9718, .T. ) ;
#15100 = CARTESIAN_POINT ( 'NONE',  ( 1.981854314971675413, -6.155463562373256536, -2.968431064909258232 ) ) ;
#15101 = CARTESIAN_POINT ( 'NONE',  ( 1.493882881115753847, -0.7724999999999562217, -3.610279343491855641 ) ) ;
#15102 = EDGE_CURVE ( 'NONE', #13967, #5514, #7492, .T. ) ;
#15103 = CARTESIAN_POINT ( 'NONE',  ( -3.466497813382189541, -5.275048774667015827, -7.182839392716466875E-16 ) ) ;
#15104 = CARTESIAN_POINT ( 'NONE',  ( 0.3952026422296860964, -2.765624999999906741, 3.997656568947202338 ) ) ;
#15105 = DIRECTION ( 'NONE',  ( 0.000000000000000000, -0.000000000000000000, 1.000000000000000000 ) ) ;
#15106 = EDGE_CURVE ( 'NONE', #14347, #13430, #9788, .T. ) ;
#15107 = EDGE_CURVE ( 'NONE', #8660, #9779, #7710, .T. ) ;
#15108 = CARTESIAN_POINT ( 'NONE',  ( -0.2824495906440828152, 2.041549731959705837E-17, 21.57312693144813665 ) ) ;
#15109 = DIRECTION ( 'NONE',  ( -1.000000000000000000, -1.067522139062645149E-15, 0.000000000000000000 ) ) ;
#15110 = CARTESIAN_POINT ( 'NONE',  ( -86.77438362644001302, 65.17411849586700612, -145.4984795835769660 ) ) ;
#15111 = CARTESIAN_POINT ( 'NONE',  ( -37.27438362644220149, 104.6741184958692088, -79.59847958357700293 ) ) ;
#15112 = PLANE ( 'NONE',  #8749 ) ;
#15113 = ORIENTED_EDGE ( 'NONE', *, *, #11417, .T. ) ;
#15114 = CARTESIAN_POINT ( 'NONE',  ( -69.77438362644001302, 82.17411849586700612, -80.14847958357698587 ) ) ;
#15115 = ORIENTED_EDGE ( 'NONE', *, *, #4658, .F. ) ;
#15116 = ADVANCED_FACE ( 'NONE', ( #7486 ), #6332, .F. ) ;
#15117 = ORIENTED_EDGE ( 'NONE', *, *, #5038, .T. ) ;
#15118 = ORIENTED_EDGE ( 'NONE', *, *, #4472, .F. ) ;
#15119 = FACE_BOUND ( 'NONE', #1632, .T. ) ;
#15120 = CARTESIAN_POINT ( 'NONE',  ( 1.903042727507366250, -4.428749999999965326, 2.845810502761935368 ) ) ;
#15121 = ADVANCED_FACE ( 'NONE', ( #10472 ), #15199, .F. ) ;
#15122 = CARTESIAN_POINT ( 'NONE',  ( -82.52438362644100778, 99.17411849586700612, -182.2484795835770228 ) ) ;
#15123 = CARTESIAN_POINT ( 'NONE',  ( -48.52438362644100067, 99.17411849586700612, -145.4984795835769944 ) ) ;
#15124 = LINE ( 'NONE', #9237, #14180 ) ;
#15125 = DIRECTION ( 'NONE',  ( -1.000000000000000000, 0.000000000000000000, 0.000000000000000000 ) ) ;
#15126 = VECTOR ( 'NONE', #1599, 1000.000000000000114 ) ;
#15127 = DIRECTION ( 'NONE',  ( -0.8660254037844387076, -0.4999999999999998890, 0.000000000000000000 ) ) ;
#15128 = DIRECTION ( 'NONE',  ( 0.000000000000000000, 0.000000000000000000, -1.000000000000000000 ) ) ;
#15129 = DIRECTION ( 'NONE',  ( -0.9961946980917453232, 7.200509705930738460E-17, -0.08715574274766157981 ) ) ;
#15130 = VECTOR ( 'NONE', #4225, 1000.000000000000000 ) ;
#15131 = VERTEX_POINT ( 'NONE', #10239 ) ;
#15132 = DIRECTION ( 'NONE',  ( -0.9961946980917452121, 7.200509705930738460E-17, -0.08715574274766156593 ) ) ;
#15133 = VERTEX_POINT ( 'NONE', #12518 ) ;
#15134 = EDGE_LOOP ( 'NONE', ( #3552, #7597, #6863, #14540 ) ) ;
#15135 = LINE ( 'NONE', #3362, #5002 ) ;
#15136 = ORIENTED_EDGE ( 'NONE', *, *, #5666, .T. ) ;
#15137 = VECTOR ( 'NONE', #3753, 1000.000000000000000 ) ;
#15138 = CARTESIAN_POINT ( 'NONE',  ( -1.643569066580401916, -0.6875000000000854872, 3.964934652274553439 ) ) ;
#15139 = ORIENTED_EDGE ( 'NONE', *, *, #3660, .F. ) ;
#15140 = CARTESIAN_POINT ( 'NONE',  ( 2.202232363153947770, -3.155463562373067798, -3.298474133106217288 ) ) ;
#15141 =( GEOMETRIC_REPRESENTATION_CONTEXT ( 3 ) GLOBAL_UNCERTAINTY_ASSIGNED_CONTEXT ( ( #1724 ) ) GLOBAL_UNIT_ASSIGNED_CONTEXT ( ( #10709, #12974, #161 ) ) REPRESENTATION_CONTEXT ( 'NONE', 'WORKASPACE' ) );
#15142 = DIRECTION ( 'NONE',  ( 0.000000000000000000, 0.000000000000000000, 1.000000000000000000 ) ) ;
#15143 = AXIS2_PLACEMENT_3D ( 'NONE', #9429, #14168, #3545 ) ;
#15144 = CARTESIAN_POINT ( 'NONE',  ( -67.09329877327367342, 89.83357606928383632, -58.65793715699378197 ) ) ;
#15145 = CARTESIAN_POINT ( 'NONE',  ( 15.50000000000000000, -0.1999999999999999556, 23.94999999999999574 ) ) ;
#15146 = CIRCLE ( 'NONE', #14412, 4.250000000000003553 ) ;
#15147 = DIRECTION ( 'NONE',  ( 1.000000000000000000, 0.000000000000000000, 0.000000000000000000 ) ) ;
#15148 = VERTEX_POINT ( 'NONE', #4363 ) ;
#15149 = DIRECTION ( 'NONE',  ( -1.000000000000000000, -2.551930889570659960E-15, 0.000000000000000000 ) ) ;
#15150 = CARTESIAN_POINT ( 'NONE',  ( 17.18164641901421419, -3.654316742536411589, 0.2664120436859910845 ) ) ;
#15151 = AXIS2_PLACEMENT_3D ( 'NONE', #8319, #13976, #14058 ) ;
#15152 = ORIENTED_EDGE ( 'NONE', *, *, #15012, .F. ) ;
#15153 = DIRECTION ( 'NONE',  ( 0.000000000000000000, 0.000000000000000000, 1.000000000000000000 ) ) ;
#15154 = CARTESIAN_POINT ( 'NONE',  ( 3.459076575081828864, -0.6631250000000769029, -1.847748348019894848 ) ) ;
#15155 = ORIENTED_EDGE ( 'NONE', *, *, #9961, .T. ) ;
#15156 = EDGE_CURVE ( 'NONE', #3619, #8760, #13174, .T. ) ;
#15157 = AXIS2_PLACEMENT_3D ( 'NONE', #9603, #2550, #3794 ) ;
#15158 = CARTESIAN_POINT ( 'NONE',  ( -3.566427039428707868, -2.131875000000089670, 1.083295335393480219 ) ) ;
#15159 = CARTESIAN_POINT ( 'NONE',  ( -50.27438362644099357, 99.17411849586700612, -182.2484795835770228 ) ) ;
#15160 = CIRCLE ( 'NONE', #14926, 0.9999999999999956701 ) ;
#15161 = CARTESIAN_POINT ( 'NONE',  ( -8.108964177917338034, 5.861171052203404620E-16, 53.66203178395558382 ) ) ;
#15162 = DIRECTION ( 'NONE',  ( 0.000000000000000000, -1.000000000000000000, 0.000000000000000000 ) ) ;
#15163 = DIRECTION ( 'NONE',  ( -1.000000000000000000, 0.000000000000000000, 0.000000000000000000 ) ) ;
#15164 = DIRECTION ( 'NONE',  ( 0.4999999999999827360, 0.000000000000000000, -0.8660254037844485886 ) ) ;
#15165 = VECTOR ( 'NONE', #8891, 1000.000000000000114 ) ;
#15166 = VERTEX_POINT ( 'NONE', #4587 ) ;
#15167 = DIRECTION ( 'NONE',  ( -1.000000000000000000, 0.000000000000000000, 0.000000000000000000 ) ) ;
#15168 = PRODUCT_DEFINITION ( 'UNKNOWN', '', #11884, #12285 ) ;
#15169 = EDGE_CURVE ( 'NONE', #10998, #7322, #938, .T. ) ;
#15170 = EDGE_LOOP ( 'NONE', ( #9046, #4777 ) ) ;
#15171 = EDGE_LOOP ( 'NONE', ( #5614, #10295, #4414, #1692, #11796 ) ) ;
#15172 = CARTESIAN_POINT ( 'NONE',  ( 3.009749400183385326, -4.506874999999939568, 1.609730366092140708 ) ) ;
#15173 = ORIENTED_EDGE ( 'NONE', *, *, #119, .F. ) ;
#15174 = EDGE_LOOP ( 'NONE', ( #6681, #7014 ) ) ;
#15175 = VECTOR ( 'NONE', #5880, 1000.000000000000000 ) ;
#15176 = ADVANCED_FACE ( 'NONE', ( #6926 ), #1955, .F. ) ;
#15177 = VECTOR ( 'NONE', #8701, 1000.000000000000000 ) ;
#15178 = EDGE_LOOP ( 'NONE', ( #470, #12454 ) ) ;
#15179 = CARTESIAN_POINT ( 'NONE',  ( 2.432356863550838355, -4.139838562373138409, -2.966048421176934458 ) ) ;
#15180 = CARTESIAN_POINT ( 'NONE',  ( 1.515516452534992897, -0.3975000000001072675, 3.655012690611888715 ) ) ;
#15181 = VECTOR ( 'NONE', #2403, 1000.000000000000000 ) ;
#15182 =( BOUNDED_CURVE ( )  B_SPLINE_CURVE ( 3, ( #12724, #5834, #1080, #1946 ),
 .UNSPECIFIED., .F., .T. ) 
 B_SPLINE_CURVE_WITH_KNOTS ( ( 4, 4 ),
 ( 6.195245264107405170, 6.283185307179586232 ),
 .UNSPECIFIED. ) 
 CURVE ( )  GEOMETRIC_REPRESENTATION_ITEM ( )  RATIONAL_B_SPLINE_CURVE ( ( 1.000000000000000000, 0.9993556495590054656, 0.9993556495590054656, 1.000000000000000000 ) ) 
 REPRESENTATION_ITEM ( '' )  );
#15183 = CARTESIAN_POINT ( 'NONE',  ( -1.169542390366794304, -2.703125000000013323, 3.851808151836873861 ) ) ;
#15184 = LINE ( 'NONE', #12878, #9725 ) ;
#15185 = LINE ( 'NONE', #9216, #11317 ) ;
#15186 = CARTESIAN_POINT ( 'NONE',  ( 3.663887442738342770, 2.356280171323993589, 2.653960795963570707 ) ) ;
#15187 = DIRECTION ( 'NONE',  ( -1.000000000000000000, 0.000000000000000000, 0.000000000000000000 ) ) ;
#15188 = LINE ( 'NONE', #10698, #14011 ) ;
#15189 = AXIS2_PLACEMENT_3D ( 'NONE', #11052, #5166, #8714 ) ;
#15190 = AXIS2_PLACEMENT_3D ( 'NONE', #11314, #14865, #1626 ) ;
#15191 = PLANE ( 'NONE',  #6730 ) ;
#15192 = DIRECTION ( 'NONE',  ( 1.445602896647339163E-16, -1.000000000000000000, 0.000000000000000000 ) ) ;
#15193 = ORIENTED_EDGE ( 'NONE', *, *, #11728, .T. ) ;
#15194 = CARTESIAN_POINT ( 'NONE',  ( -35.58670980944424400, 5.000000000000000000, 129.5095611191910621 ) ) ;
#15195 = ORIENTED_EDGE ( 'NONE', *, *, #2292, .F. ) ;
#15196 = ORIENTED_EDGE ( 'NONE', *, *, #2029, .T. ) ;
#15197 = ORIENTED_EDGE ( 'NONE', *, *, #3942, .T. ) ;
#15198 = EDGE_CURVE ( 'NONE', #9914, #5515, #6267, .T. ) ;
#15199 = PLANE ( 'NONE',  #13431 ) ;
#15200 = EDGE_CURVE ( 'NONE', #11747, #6469, #13675, .T. ) ;
#15201 = AXIS2_PLACEMENT_3D ( 'NONE', #5039, #14568, #14487 ) ;
#15202 = CARTESIAN_POINT ( 'NONE',  ( -50.27438362644100067, 59.67411849586700612, -79.59847958357700293 ) ) ;
#15203 = LINE ( 'NONE', #13755, #5018 ) ;
#15204 = CARTESIAN_POINT ( 'NONE',  ( -59.02799568714584666, 164.3482369917340122, -73.34256232478206528 ) ) ;
#15205 = CARTESIAN_POINT ( 'NONE',  ( -86.77438362644001302, 99.17411849586700612, -86.49847958357699440 ) ) ;
#15206 = ADVANCED_FACE ( 'NONE', ( #13829 ), #4283, .F. ) ;
#15207 = DIRECTION ( 'NONE',  ( 0.000000000000000000, 1.000000000000000000, 0.000000000000000000 ) ) ;
#15208 = CARTESIAN_POINT ( 'NONE',  ( 4.330127018922191873, 1.087837616813861542E-14, -1.500000000000001332 ) ) ;
#15209 = DIRECTION ( 'NONE',  ( 0.9961946980917453232, -8.673617379884040205E-15, 0.08715574274766051122 ) ) ;
#15210 = LINE ( 'NONE', #6244, #1572 ) ;
#15211 = ORIENTED_EDGE ( 'NONE', *, *, #14333, .T. ) ;
#15212 = DIRECTION ( 'NONE',  ( -0.000000000000000000, -0.000000000000000000, 1.000000000000000000 ) ) ;
#15213 = AXIS2_PLACEMENT_3D ( 'NONE', #7222, #1312, #6076 ) ;
#15214 = AXIS2_PLACEMENT_3D ( 'NONE', #13329, #2606, #11073 ) ;
#15215 = ADVANCED_FACE ( 'NONE', ( #10393 ), #11412, .F. ) ;
#15216 = EDGE_LOOP ( 'NONE', ( #12904, #11969, #5670, #2160 ) ) ;
#15217 = ORIENTED_EDGE ( 'NONE', *, *, #11042, .F. ) ;
#15218 = PLANE ( 'NONE',  #8214 ) ;
#15219 = ORIENTED_EDGE ( 'NONE', *, *, #6246, .T. ) ;
#15220 = EDGE_CURVE ( 'NONE', #15299, #10086, #780, .T. ) ;
#15221 = EDGE_CURVE ( 'NONE', #5866, #4720, #1075, .T. ) ;
#15222 = ORIENTED_EDGE ( 'NONE', *, *, #2619, .F. ) ;
#15223 = CARTESIAN_POINT ( 'NONE',  ( 4.035539303778883813, -2.030463562373035380, -0.8042393191121177676 ) ) ;
#15224 = FACE_OUTER_BOUND ( 'NONE', #14136, .T. ) ;
#15225 = DIRECTION ( 'NONE',  ( 0.000000000000000000, 0.000000000000000000, -1.000000000000000000 ) ) ;
#15226 = AXIS2_PLACEMENT_3D ( 'NONE', #14656, #4041, #6087 ) ;
#15227 = CARTESIAN_POINT ( 'NONE',  ( -88.81638362644000040, 63.99516924618178848, -147.9984795835769944 ) ) ;
#15228 = VECTOR ( 'NONE', #10228, 1000.000000000000114 ) ;
#15229 = CARTESIAN_POINT ( 'NONE',  ( -69.77438362644001302, 82.17411849586700612, -29.37106258560738681 ) ) ;
#15230 = ORIENTED_EDGE ( 'NONE', *, *, #40, .F. ) ;
#15231 = DIRECTION ( 'NONE',  ( -1.000000000000000000, -0.000000000000000000, -0.000000000000000000 ) ) ;
#15232 = LINE ( 'NONE', #11836, #4277 ) ;
#15233 = AXIS2_PLACEMENT_3D ( 'NONE', #1983, #6811, #11452 ) ;
#15234 = ORIENTED_EDGE ( 'NONE', *, *, #4142, .F. ) ;
#15235 = CARTESIAN_POINT ( 'NONE',  ( -15.50000000000000000, -0.2038245569916614930, 21.05662432702600029 ) ) ;
#15236 = CARTESIAN_POINT ( 'NONE',  ( 3.104176526174651229, -4.906250000000120792, 2.075311058921220919 ) ) ;
#15237 = VERTEX_POINT ( 'NONE', #5620 ) ;
#15238 = AXIS2_PLACEMENT_3D ( 'NONE', #1622, #11311, #12562 ) ;
#15239 = CARTESIAN_POINT ( 'NONE',  ( -0.3703630857574056745, -1.850625000000086340, -3.746264557426716379 ) ) ;
#15240 = CARTESIAN_POINT ( 'NONE',  ( 0.000000000000000000, -2.500000000000000000, 0.000000000000000000 ) ) ;
#15241 = AXIS2_PLACEMENT_3D ( 'NONE', #1331, #1419, #13293 ) ;
#15242 = CARTESIAN_POINT ( 'NONE',  ( -12.81835358098578403, 11.99999970914576330, -11.73358795631400753 ) ) ;
#15243 = VECTOR ( 'NONE', #12910, 1000.000000000000000 ) ;
#15244 = FACE_OUTER_BOUND ( 'NONE', #10158, .T. ) ;
#15245 = DIRECTION ( 'NONE',  ( -0.08715574274766155205, 0.000000000000000000, 0.9961946980917452121 ) ) ;
#15246 = CIRCLE ( 'NONE', #11542, 3.300000002979700753 ) ;
#15247 = DIRECTION ( 'NONE',  ( 0.000000000000000000, 1.000000000000000000, 0.000000000000000000 ) ) ;
#15248 = FACE_OUTER_BOUND ( 'NONE', #177, .T. ) ;
#15249 = ORIENTED_EDGE ( 'NONE', *, *, #5742, .T. ) ;
#15250 = CARTESIAN_POINT ( 'NONE',  ( -86.77438362644100778, 99.17411849586700612, -145.4984795835769944 ) ) ;
#15251 = ORIENTED_EDGE ( 'NONE', *, *, #3265, .T. ) ;
#15252 = ORIENTED_EDGE ( 'NONE', *, *, #7330, .T. ) ;
#15253 = ORIENTED_EDGE ( 'NONE', *, *, #5432, .T. ) ;
#15254 = VECTOR ( 'NONE', #6280, 1000.000000000000000 ) ;
#15255 = VERTEX_POINT ( 'NONE', #7995 ) ;
#15256 = EDGE_LOOP ( 'NONE', ( #2513, #5923, #10236, #10156 ) ) ;
#15257 = AXIS2_PLACEMENT_3D ( 'NONE', #2739, #1506, #334 ) ;
#15258 = CARTESIAN_POINT ( 'NONE',  ( -3.767882347484534211, -4.514838562373170383, 0.3724990980822453501 ) ) ;
#15259 = FACE_OUTER_BOUND ( 'NONE', #11699, .T. ) ;
#15260 = LINE ( 'NONE', #9598, #14778 ) ;
#15261 = DIRECTION ( 'NONE',  ( 0.000000000000000000, 0.000000000000000000, 1.000000000000000000 ) ) ;
#15262 = ADVANCED_FACE ( 'NONE', ( #4438 ), #12734, .F. ) ;
#15263 = CARTESIAN_POINT ( 'NONE',  ( 66.41329019055578442, 5.000000000000000000, 137.5095611191910621 ) ) ;
#15264 = CARTESIAN_POINT ( 'NONE',  ( 35.35543536254876074, -3.618985300545107364, 6.000000000000001776 ) ) ;
#15265 = DIRECTION ( 'NONE',  ( 0.000000000000000000, 0.000000000000000000, -1.000000000000000000 ) ) ;
#15266 = AXIS2_PLACEMENT_3D ( 'NONE', #10419, #10586, #5885 ) ;
#15267 = FACE_OUTER_BOUND ( 'NONE', #7119, .T. ) ;
#15268 = CARTESIAN_POINT ( 'NONE',  ( 22.58164641901421632, 11.99999970914575798, -0.3335879563140091153 ) ) ;
#15269 = EDGE_CURVE ( 'NONE', #13375, #11145, #2102, .T. ) ;
#15270 = CARTESIAN_POINT ( 'NONE',  ( -2.129528971937844517, -4.944374999999755715, -2.592863122870853410 ) ) ;
#15271 = LINE ( 'NONE', #14271, #74 ) ;
#15272 = AXIS2_PLACEMENT_3D ( 'NONE', #1415, #6173, #2651 ) ;
#15273 = VERTEX_POINT ( 'NONE', #5765 ) ;
#15274 = DIRECTION ( 'NONE',  ( -1.000000000000000000, 0.000000000000000000, 0.000000000000000000 ) ) ;
#15275 = ORIENTED_EDGE ( 'NONE', *, *, #14316, .T. ) ;
#15276 = ORIENTED_EDGE ( 'NONE', *, *, #11326, .F. ) ;
#15277 = EDGE_LOOP ( 'NONE', ( #2767, #367, #13376, #10788 ) ) ;
#15278 = CARTESIAN_POINT ( 'NONE',  ( -86.77438362644100778, 101.5320169952374414, -147.9984795835769944 ) ) ;
#15279 = AXIS2_PLACEMENT_3D ( 'NONE', #3435, #2041, #10485 ) ;
#15280 = CIRCLE ( 'NONE', #12082, 2.500000000000002220 ) ;
#15281 = DIRECTION ( 'NONE',  ( -1.000000000000000000, 1.287488025362404182E-15, 0.000000000000000000 ) ) ;
#15282 = DIRECTION ( 'NONE',  ( 0.7071067811865474617, 0.000000000000000000, 0.7071067811865474617 ) ) ;
#15283 = PLANE ( 'NONE',  #2533 ) ;
#15284 = ADVANCED_FACE ( 'NONE', ( #15119, #1880 ), #6634, .T. ) ;
#15285 = DIRECTION ( 'NONE',  ( 1.224646799147351975E-16, 1.000000000000000000, 0.000000000000000000 ) ) ;
#15286 = LINE ( 'NONE', #7865, #8367 ) ;
#15287 = DIRECTION ( 'NONE',  ( 0.000000000000000000, 0.000000000000000000, -1.000000000000000000 ) ) ;
#15288 = FACE_OUTER_BOUND ( 'NONE', #12989, .T. ) ;
#15289 = ADVANCED_FACE ( 'NONE', ( #8457 ), #1241, .F. ) ;
#15290 = CARTESIAN_POINT ( 'NONE',  ( -55.52438362644000591, 65.17411849586700612, -145.4984795835769660 ) ) ;
#15291 = ORIENTED_EDGE ( 'NONE', *, *, #5571, .T. ) ;
#15292 = LINE ( 'NONE', #9245, #14052 ) ;
#15293 = EDGE_LOOP ( 'NONE', ( #14297, #3883, #8328, #9832 ) ) ;
#15294 = VECTOR ( 'NONE', #12422, 1000.000000000000000 ) ;
#15295 = ORIENTED_EDGE ( 'NONE', *, *, #319, .T. ) ;
#15296 = DIRECTION ( 'NONE',  ( -1.000000000000000000, 0.000000000000000000, 6.860497997771530774E-15 ) ) ;
#15297 = ADVANCED_FACE ( 'NONE', ( #5846 ), #2481, .F. ) ;
#15298 = LINE ( 'NONE', #2351, #13906 ) ;
#15299 = VERTEX_POINT ( 'NONE', #8313 ) ;
#15300 = EDGE_CURVE ( 'NONE', #3363, #12177, #6752, .T. ) ;
#15301 = CARTESIAN_POINT ( 'NONE',  ( 3.324617108750066663, -2.905463562373210351, 2.222704761906319160 ) ) ;
#15302 = FACE_OUTER_BOUND ( 'NONE', #5389, .T. ) ;
#15303 = ADVANCED_FACE ( 'NONE', ( #5929 ), #10874, .F. ) ;
#15304 = DIRECTION ( 'NONE',  ( 0.000000000000000000, 0.000000000000000000, 1.000000000000000000 ) ) ;
#15305 = CARTESIAN_POINT ( 'NONE',  ( -52.77438362644000591, 99.17411849586700612, -79.59847958357700293 ) ) ;
#15306 = EDGE_CURVE ( 'NONE', #382, #4318, #5266, .T. ) ;
#15307 = LINE ( 'NONE', #14082, #9495 ) ;
#15308 = ADVANCED_FACE ( 'NONE', ( #6167 ), #7159, .T. ) ;
#15309 = ORIENTED_EDGE ( 'NONE', *, *, #10666, .T. ) ;
#15310 = CARTESIAN_POINT ( 'NONE',  ( -55.27438362643999881, 65.17411849586700612, -182.2484795835770228 ) ) ;
#15311 = DIRECTION ( 'NONE',  ( 0.000000000000000000, 1.000000000000000000, 0.000000000000000000 ) ) ;
#15312 = ORIENTED_EDGE ( 'NONE', *, *, #2228, .F. ) ;
#15313 = AXIS2_PLACEMENT_3D ( 'NONE', #9426, #11924, #7047 ) ;
#15314 = FILL_AREA_STYLE_COLOUR ( '', #10283 ) ;
#15315 = CARTESIAN_POINT ( 'NONE',  ( -1.733052192687106308, -5.328125000000219380, -3.244333203286712042 ) ) ;
#15316 = EDGE_LOOP ( 'NONE', ( #2873, #6950 ) ) ;
#15317 = CARTESIAN_POINT ( 'NONE',  ( -1.439523803302256155, -1.897500000000171383, -3.471712813344601578 ) ) ;
#15318 = EDGE_CURVE ( 'NONE', #8134, #9846, #10795, .T. ) ;
#15319 = CARTESIAN_POINT ( 'NONE',  ( -47.27438362644100778, 57.67411849586700612, -67.49847958357700861 ) ) ;
#15320 = CIRCLE ( 'NONE', #6923, 0.5999999999999998668 ) ;
#15321 = DIRECTION ( 'NONE',  ( -0.3469356515732558988, 0.9378889346118975956, 0.000000000000000000 ) ) ;
#15322 = SURFACE_STYLE_FILL_AREA ( #15016 ) ;
#15323 = CARTESIAN_POINT ( 'NONE',  ( -1.733498803496028140, -12.00000029085427578, 38.15869532822594579 ) ) ;
#15324 = FACE_OUTER_BOUND ( 'NONE', #4186, .T. ) ;
#15325 = ORIENTED_EDGE ( 'NONE', *, *, #4710, .T. ) ;
#15326 = CARTESIAN_POINT ( 'NONE',  ( -102.2743836264409936, 62.67411849586699901, -79.59847958357700293 ) ) ;
#15327 = ORIENTED_EDGE ( 'NONE', *, *, #11591, .T. ) ;
#15328 = VERTEX_POINT ( 'NONE', #4825 ) ;
#15329 = CARTESIAN_POINT ( 'NONE',  ( 0.6686498792469652841, -4.366249999999815223, 3.366016213005436519 ) ) ;
#15330 = VERTEX_POINT ( 'NONE', #9387 ) ;
#15331 = ORIENTED_EDGE ( 'NONE', *, *, #15094, .F. ) ;
#15332 = ORIENTED_EDGE ( 'NONE', *, *, #7712, .T. ) ;
#15333 = CARTESIAN_POINT ( 'NONE',  ( -1.441154219919537516, -4.686713562373249431, 3.476695106718095118 ) ) ;
#15334 = DIRECTION ( 'NONE',  ( -1.000000000000000000, -1.067522139062645149E-15, 0.000000000000000000 ) ) ;
#15335 = ORIENTED_EDGE ( 'NONE', *, *, #888, .T. ) ;
#15336 = NEXT_ASSEMBLY_USAGE_OCCURRENCE ( 'NAUO1', ' ', ' ', #10143, #14892, $ ) ;
#15337 = NEXT_ASSEMBLY_USAGE_OCCURRENCE ( 'NAUO2', ' ', ' ', #10143, #15168, $ ) ;
#15338 = NEXT_ASSEMBLY_USAGE_OCCURRENCE ( 'NAUO3', ' ', ' ', #10143, #7626, $ ) ;
#15339 = NEXT_ASSEMBLY_USAGE_OCCURRENCE ( 'NAUO4', ' ', ' ', #10143, #5538, $ ) ;
#15340 = NEXT_ASSEMBLY_USAGE_OCCURRENCE ( 'NAUO5', ' ', ' ', #10143, #5538, $ ) ;
#15341 = NEXT_ASSEMBLY_USAGE_OCCURRENCE ( 'NAUO6', ' ', ' ', #10143, #3235, $ ) ;
#15342 = NEXT_ASSEMBLY_USAGE_OCCURRENCE ( 'NAUO7', ' ', ' ', #7626, #13774, $ ) ;
#15343 = NEXT_ASSEMBLY_USAGE_OCCURRENCE ( 'NAUO8', ' ', ' ', #7626, #13774, $ ) ;
#15344 = NEXT_ASSEMBLY_USAGE_OCCURRENCE ( 'NAUO9', ' ', ' ', #7626, #7428, $ ) ;
ENDSEC;
END-ISO-10303-21;
